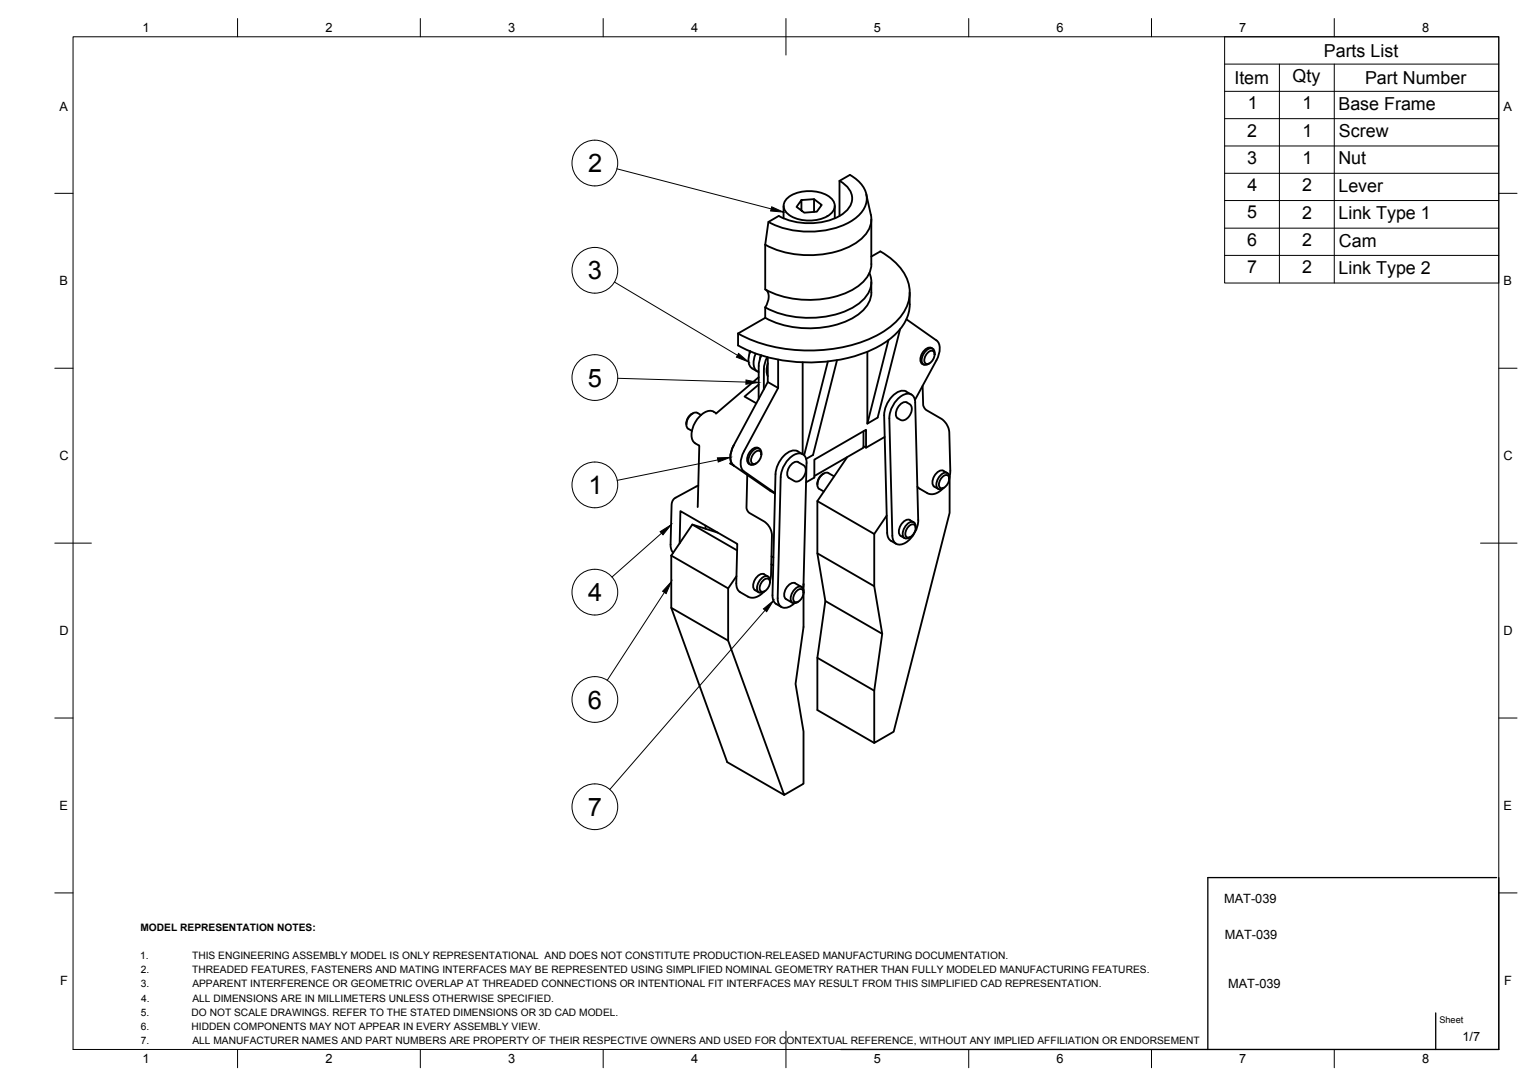
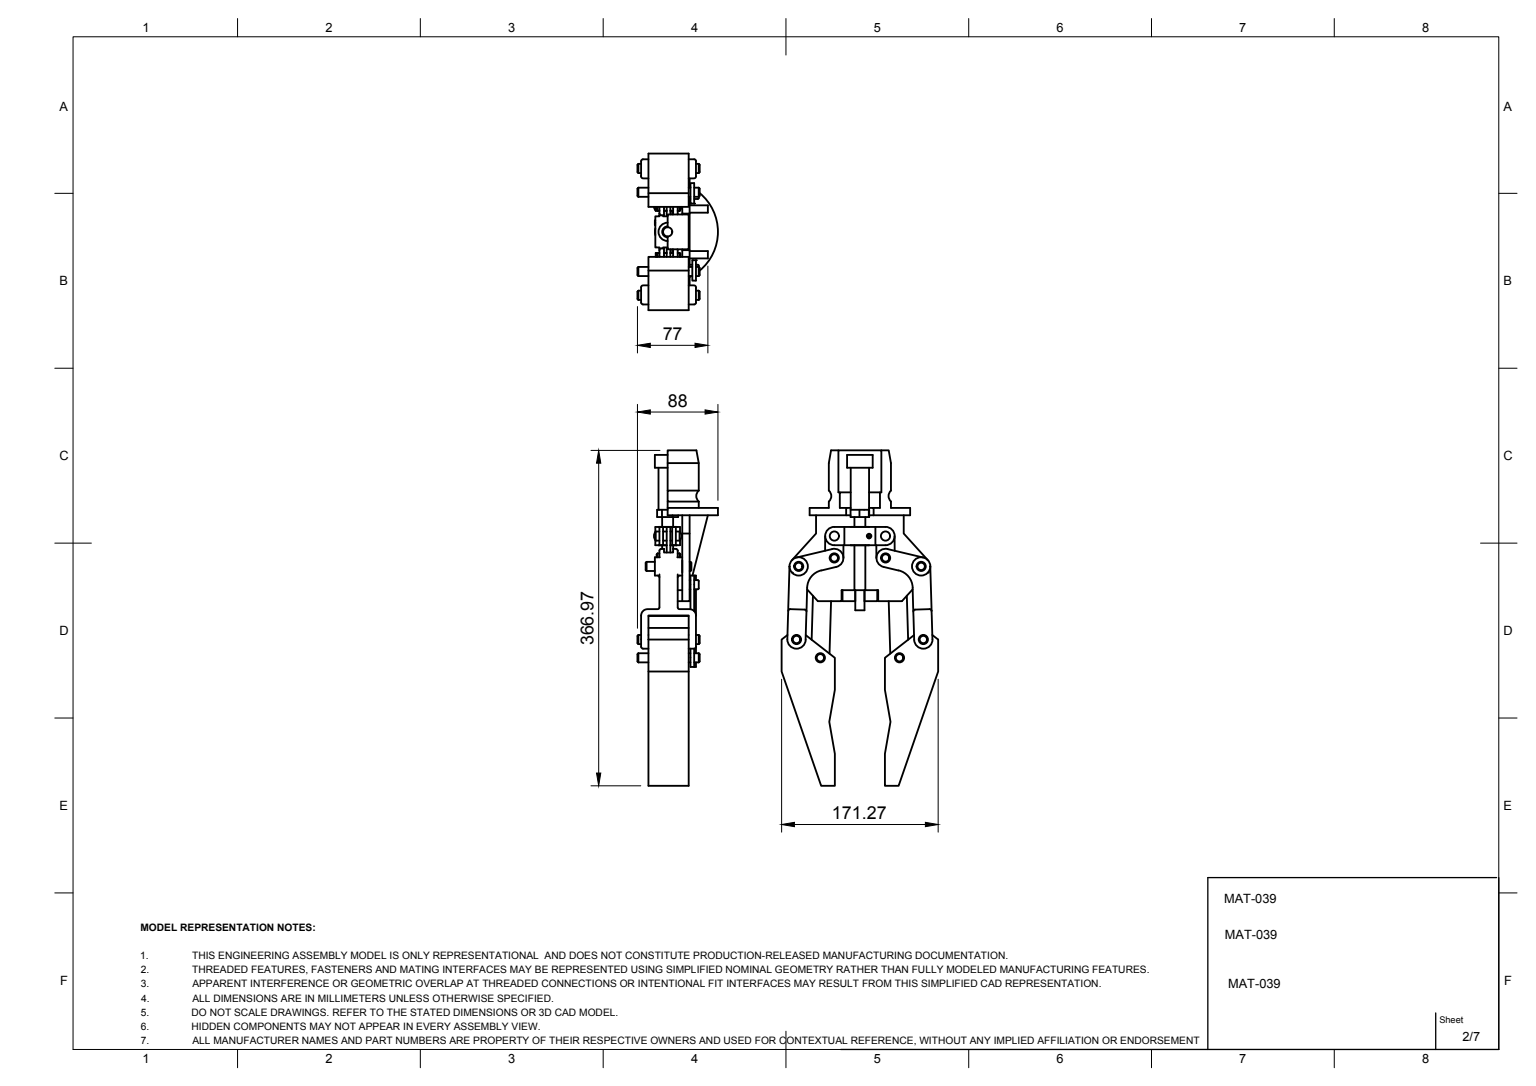
ISO-10303-21;
HEADER;
/* Generated by software containing ST-Developer
 * from STEP Tools, Inc. (www.steptools.com) 
 */

FILE_DESCRIPTION(
/* description */ ('STEP AP214'),
/* implementation_level */ '2;1');

FILE_NAME(
/* name */ 'MAT-039.step',
/* time_stamp */ '2026-11-14T21:46:24-08:00',
/* author */ (''),
/* organization */ (''),
/* preprocessor_version */ 'ST-DEVELOPER v20.2',
/* originating_system */ 'Autodesk Translation Framework v15.17.0.0',
/* authorisation */ '');

FILE_SCHEMA (('AUTOMOTIVE_DESIGN { 1 0 10303 214 3 1 1 }'));
ENDSEC;

DATA;
#10=MECHANICAL_DESIGN_GEOMETRIC_PRESENTATION_REPRESENTATION('',(#89,#90,
#91,#92,#93,#94,#95),#7783);
#11=(
BOUNDED_SURFACE()
B_SPLINE_SURFACE(3,2,((#7242,#7243,#7244),(#7245,#7246,#7247),(#7248,#7249,
#7250),(#7251,#7252,#7253),(#7254,#7255,#7256),(#7257,#7258,#7259),(#7260,
#7261,#7262),(#7263,#7264,#7265),(#7266,#7267,#7268),(#7269,#7270,#7271),
(#7272,#7273,#7274),(#7275,#7276,#7277),(#7278,#7279,#7280),(#7281,#7282,
#7283)),.UNSPECIFIED.,.F.,.F.,.F.)
B_SPLINE_SURFACE_WITH_KNOTS((4,2,2,2,2,2,4),(3,3),(0.00201286221565559,
0.00340012561105001,0.00476544226438698,0.00613075891772395,0.00749607557106092,
0.0102267088777349,0.0129573421844088),(0.,1.00002194674206),
 .UNSPECIFIED.)
GEOMETRIC_REPRESENTATION_ITEM()
RATIONAL_B_SPLINE_SURFACE(((1.,0.706119316799645,1.0000128994471),(1.,0.726784777924549,
1.00001199236801),(1.,0.747777874428932,1.00001107090786),(1.,0.788599708818028,
1.00000927909532),(1.,0.808519289419434,1.00000840475553),(1.,0.845529525851375,
1.0000067802473),(1.,0.862790936611022,1.00000602258384),(1.,0.894561465950779,
1.00000462806462),(1.,0.909105255838781,1.00000398968701),(1.,0.948117278028828,
1.00000227731343),(1.,0.967426794359605,1.00000142975148),(1.,0.993377057003404,
1.00000029070404),(1.,0.999996114407628,1.00000000017055),(1.,1.,1.)))
REPRESENTATION_ITEM('')
SURFACE()
);
#12=(
BOUNDED_SURFACE()
B_SPLINE_SURFACE(3,2,((#7288,#7289,#7290),(#7291,#7292,#7293),(#7294,#7295,
#7296),(#7297,#7298,#7299),(#7300,#7301,#7302),(#7303,#7304,#7305),(#7306,
#7307,#7308),(#7309,#7310,#7311),(#7312,#7313,#7314),(#7315,#7316,#7317),
(#7318,#7319,#7320),(#7321,#7322,#7323),(#7324,#7325,#7326),(#7327,#7328,
#7329)),.UNSPECIFIED.,.F.,.F.,.F.)
B_SPLINE_SURFACE_WITH_KNOTS((4,2,2,2,2,2,4),(3,3),(0.00201286221604104,
0.00340012561105,0.00476544226438698,0.00613075891772395,0.00749607557106092,
0.0102267088777349,0.0129573421844088),(-2.19467416719971E-5,1.00004202921769),
 .UNSPECIFIED.)
GEOMETRIC_REPRESENTATION_ITEM()
RATIONAL_B_SPLINE_SURFACE(((1.00001289944687,0.706106964970707,1.00002470364651),
(1.0000119923678,0.726773294662226,1.00002296650529),(1.00001107090767,
0.747767273503531,1.00002120182301),(1.00000927909516,0.788590823634209,
1.00001777033457),(1.00000840475538,0.808511241458396,1.00001609589217),
(1.00000678024718,0.845523033435795,1.00001298480712),(1.00000602258374,
0.862785169694921,1.00001153381081),(1.00000462806454,0.894557034354464,
1.00000886317619),(1.00000398968694,0.909101435519961,1.00000764062341),
(1.00000227731339,0.948115097390828,1.00000436126801),(1.00000142975146,
0.967425425303272,1.00000273810769),(1.00000029070404,0.993376778640135,
1.00000055672541),(1.00000000017055,0.999996114244353,1.00000000032662),
(1.,1.,1.)))
REPRESENTATION_ITEM('')
SURFACE()
);
#13=(
BOUNDED_SURFACE()
B_SPLINE_SURFACE(3,2,((#7444,#7445,#7446),(#7447,#7448,#7449),(#7450,#7451,
#7452),(#7453,#7454,#7455),(#7456,#7457,#7458),(#7459,#7460,#7461),(#7462,
#7463,#7464),(#7465,#7466,#7467),(#7468,#7469,#7470),(#7471,#7472,#7473),
(#7474,#7475,#7476),(#7477,#7478,#7479),(#7480,#7481,#7482),(#7483,#7484,
#7485)),.UNSPECIFIED.,.F.,.F.,.F.)
B_SPLINE_SURFACE_WITH_KNOTS((4,2,2,2,2,2,4),(3,3),(0.00203480895771304,
0.00340012561105001,0.00476544226438698,0.00613075891772395,0.00749607557106092,
0.0102267088777349,0.0129573421844088),(0.,1.),.UNSPECIFIED.)
GEOMETRIC_REPRESENTATION_ITEM()
RATIONAL_B_SPLINE_SURFACE(((1.,0.707106781186548,1.),(1.,0.727454883115531,
1.),(1.,0.748108881352396,1.),(1.,0.788604348263869,1.),(1.,0.808523491704972,
1.),(1.,0.845532915900626,1.),(1.,0.862793947836832,1.),(1.,0.89456377993233,
1.),(1.,0.909107250638557,1.),(1.,0.948118416660453,1.),(1.,0.967427509219659,
1.),(1.,0.993377202352236,1.),(1.,0.999996114492902,1.),(1.,1.,1.)))
REPRESENTATION_ITEM('')
SURFACE()
);
#14=(
BOUNDED_SURFACE()
B_SPLINE_SURFACE(3,2,((#7492,#7493,#7494),(#7495,#7496,#7497),(#7498,#7499,
#7500),(#7501,#7502,#7503),(#7504,#7505,#7506),(#7507,#7508,#7509),(#7510,
#7511,#7512),(#7513,#7514,#7515),(#7516,#7517,#7518),(#7519,#7520,#7521),
(#7522,#7523,#7524),(#7525,#7526,#7527),(#7528,#7529,#7530),(#7531,#7532,
#7533)),.UNSPECIFIED.,.F.,.F.,.F.)
B_SPLINE_SURFACE_WITH_KNOTS((4,2,2,2,2,2,4),(3,3),(0.00203480895771304,
0.00340012561105001,0.00476544226438698,0.00613075891772395,0.00749607557106092,
0.0102267088777349,0.0129573421844088),(-4.20282077345397E-5,1.),
 .UNSPECIFIED.)
GEOMETRIC_REPRESENTATION_ITEM()
RATIONAL_B_SPLINE_SURFACE(((1.0000246205888,0.707094471409503,1.),(1.00002291012841,
0.727443428532761,1.),(1.00002117395439,0.74809829482011,1.),(1.00001776990754,
0.788595463683529,1.),(1.00001609550537,0.808515444290505,1.),(1.00001298449509,
0.845526423925928,1.),(1.00001153353364,0.862788181312395,1.),(1.0000088629632,
0.894559348636945,1.),(1.0000076404398,0.909103430579154,1.),(1.00000436116321,
0.948116236170593,1.),(1.00000273804189,0.967426140256249,1.),(1.00000055671203,
0.99337692400792,1.),(1.00000000032662,0.999996114329601,1.),(1.,1.,1.)))
REPRESENTATION_ITEM('')
SURFACE()
);
#15=B_SPLINE_CURVE_WITH_KNOTS('',3,(#6784,#6785,#6786,#6787,#6788,#6789,
#6790,#6791,#6792,#6793,#6794,#6795,#6796,#6797,#6798,#6799,#6800,#6801,
#6802,#6803,#6804,#6805,#6806,#6807,#6808,#6809,#6810,#6811,#6812,#6813,
#6814,#6815,#6816,#6817,#6818,#6819,#6820,#6821,#6822,#6823,#6824,#6825,
#6826,#6827,#6828,#6829,#6830,#6831,#6832),.UNSPECIFIED.,.F.,.F.,(4,3,3,
3,3,3,3,3,3,3,3,3,3,3,3,3,4),(0.,0.000463967413666575,0.000954777042109378,
0.00114718345131556,0.00157257184718515,0.0019889538699822,0.00230336685082165,
0.00277738225277823,0.00314514369437031,0.0034731976359017,0.00393142961796289,
0.00434870227875263,0.00465308895983082,0.00471771554155546,0.00539019410311121,
0.00607303876857302,0.00629028738874061),.UNSPECIFIED.);
#16=B_SPLINE_CURVE_WITH_KNOTS('',3,(#6834,#6835,#6836,#6837,#6838,#6839),
 .UNSPECIFIED.,.F.,.F.,(4,2,4),(0.00629028738874061,0.0078707452346593,
0.00945120308057799),.UNSPECIFIED.);
#17=B_SPLINE_CURVE_WITH_KNOTS('',3,(#6843,#6844,#6845,#6846,#6847,#6848),
 .UNSPECIFIED.,.F.,.F.,(4,2,4),(-2.00176139701977E-5,0.00156468827612987,
0.00314939416622993),.UNSPECIFIED.);
#18=B_SPLINE_CURVE_WITH_KNOTS('',3,(#6849,#6850,#6851,#6852,#6853,#6854,
#6855,#6856,#6857,#6858,#6859,#6860,#6861,#6862,#6863,#6864,#6865,#6866,
#6867,#6868,#6869,#6870,#6871,#6872,#6873,#6874,#6875,#6876,#6877,#6878,
#6879,#6880,#6881,#6882,#6883,#6884,#6885,#6886,#6887,#6888,#6889,#6890,
#6891,#6892,#6893,#6894,#6895,#6896,#6897),.UNSPECIFIED.,.F.,.F.,(4,3,3,
3,3,3,3,3,3,3,3,3,3,3,3,3,4),(0.00314939416622993,0.00383486824301925,0.00450997916923667,
0.00472621979976512,0.00479102119555099,0.00520942257342087,0.00551463261653271,
0.00597410411013286,0.0063030454333003,0.0067783430407421,0.00714709927223923,
0.00756460760297828,0.00787987106683548,0.0083064101327715,0.00880180611055996,
0.00926887465145742,0.00945669670037066),.UNSPECIFIED.);
#19=B_SPLINE_CURVE_WITH_KNOTS('',3,(#6902,#6903,#6904,#6905,#6906,#6907,
#6908,#6909,#6910,#6911,#6912,#6913,#6914,#6915,#6916,#6917,#6918,#6919,
#6920,#6921,#6922,#6923,#6924,#6925,#6926,#6927,#6928,#6929,#6930,#6931,
#6932,#6933,#6934,#6935,#6936,#6937,#6938,#6939,#6940,#6941,#6942,#6943,
#6944,#6945,#6946,#6947,#6948,#6949,#6950,#6951,#6952,#6953,#6954,#6955,
#6956,#6957,#6958,#6959,#6960,#6961,#6962,#6963,#6964,#6965,#6966,#6967,
#6968),.UNSPECIFIED.,.F.,.F.,(4,3,3,3,3,3,3,3,3,3,3,3,3,3,3,3,3,3,3,3,3,
3,4),(0.,0.000573434007013873,0.00114686801402775,0.00118140038507225,0.00174268388294295,
0.00230396738081366,0.0023628007701445,0.00306787423031747,0.00347315409373973,
0.00354420115521674,0.0040039106218915,0.0044814901760133,0.00465309204256514,
0.00472560154028899,0.00565974635025426,0.00664141956317292,0.00704595844743703,
0.00708840231043349,0.0077443311007397,0.00826980269550574,0.00881956648446386,
0.00937303729633357,0.00945120308057799),.UNSPECIFIED.);
#20=B_SPLINE_CURVE_WITH_KNOTS('',3,(#6972,#6973,#6974,#6975,#6976,#6977,
#6978,#6979,#6980,#6981,#6982,#6983,#6984,#6985,#6986,#6987,#6988,#6989,
#6990,#6991,#6992,#6993,#6994,#6995,#6996,#6997,#6998,#6999,#7000,#7001,
#7002,#7003,#7004,#7005,#7006,#7007,#7008,#7009,#7010,#7011,#7012,#7013,
#7014,#7015,#7016,#7017,#7018,#7019,#7020,#7021,#7022,#7023,#7024,#7025,
#7026,#7027,#7028,#7029,#7030,#7031,#7032,#7033,#7034,#7035),
 .UNSPECIFIED.,.F.,.F.,(4,3,3,3,3,3,3,3,3,3,3,3,3,3,3,3,3,3,3,3,3,4),(-2.00176139701506E-5,
0.000743071051629322,0.00154611600812219,0.00230505274395684,0.00234916096461506,
0.00239167902346657,0.00338088357647153,0.00432175791491912,0.00471833954320027,
0.00479101813919611,0.0052714217586875,0.00573373183999769,0.00590292883249288,
0.00597414776682822,0.00668110904687163,0.00708751812178548,0.00714649712036357,
0.00770930226572083,0.00827210741107809,0.00830672642201829,0.00888171156119449,
0.0094566967003707),.UNSPECIFIED.);
#21=B_SPLINE_CURVE_WITH_KNOTS('',3,(#7224,#7225,#7226,#7227,#7228,#7229,
#7230,#7231,#7232,#7233,#7234,#7235,#7236,#7237,#7238,#7239),
 .UNSPECIFIED.,.F.,.F.,(4,2,2,2,2,2,2,4),(0.,0.0011867209290651,0.0023734418581302,
0.00356016278719531,0.00474688371626041,0.00712032557439061,0.00830704650345571,
0.00949376743252081),.UNSPECIFIED.);
#22=B_SPLINE_CURVE_WITH_KNOTS('',3,(#7330,#7331,#7332,#7333,#7334,#7335,
#7336,#7337,#7338,#7339,#7340,#7341,#7342,#7343,#7344,#7345),
 .UNSPECIFIED.,.F.,.F.,(4,2,2,2,2,2,2,4),(0.,0.0011867209290651,0.00237344185813019,
0.00356016278719529,0.00474688371626039,0.00712032557439059,0.00830704650345569,
0.00949376743252079),.UNSPECIFIED.);
#23=B_SPLINE_CURVE_WITH_KNOTS('',3,(#7372,#7373,#7374,#7375,#7376,#7377,
#7378,#7379,#7380,#7381,#7382,#7383,#7384,#7385,#7386,#7387,#7388,#7389,
#7390,#7391,#7392,#7393,#7394,#7395,#7396,#7397,#7398,#7399,#7400,#7401,
#7402,#7403,#7404,#7405,#7406,#7407,#7408,#7409,#7410,#7411,#7412,#7413,
#7414,#7415,#7416,#7417,#7418,#7419,#7420,#7421,#7422,#7423,#7424,#7425,
#7426,#7427,#7428,#7429,#7430,#7431,#7432,#7433,#7434,#7435,#7436,#7437,
#7438,#7439,#7440,#7441),.UNSPECIFIED.,.F.,.F.,(4,3,3,3,3,3,3,3,3,3,3,3,
3,3,3,3,3,3,3,3,3,3,3,4),(-2.20338883785527E-5,0.000642558597019686,0.00116395721593939,
0.00201707586197036,0.00234994832025733,0.00244440929736401,0.00317109830627835,
0.00387836420487405,0.00455999932782322,0.00472193052889321,0.00487208598317901,
0.00547292850863629,0.00607377103409357,0.00663117903387144,0.00709391273752908,
0.00724862880926105,0.00759056213579682,0.00791199062197989,0.0082104406191189,
0.00827990384184702,0.00838782827049795,0.00882409089832456,0.00926054923459336,
0.00946589494616496),.UNSPECIFIED.);
#24=B_SPLINE_CURVE_WITH_KNOTS('',3,(#7534,#7535,#7536,#7537,#7538,#7539,
#7540,#7541,#7542,#7543,#7544,#7545,#7546,#7547,#7548,#7549,#7550,#7551,
#7552,#7553,#7554,#7555,#7556,#7557,#7558,#7559,#7560,#7561,#7562,#7563,
#7564,#7565,#7566,#7567,#7568,#7569,#7570,#7571,#7572,#7573,#7574,#7575,
#7576,#7577,#7578,#7579,#7580,#7581,#7582,#7583,#7584,#7585,#7586,#7587,
#7588,#7589,#7590,#7591,#7592,#7593,#7594,#7595,#7596,#7597,#7598,#7599,
#7600,#7601,#7602,#7603),.UNSPECIFIED.,.F.,.F.,(4,3,3,3,3,3,3,3,3,3,3,3,
3,3,3,3,3,3,3,3,3,3,3,4),(-2.20338883785244E-5,0.000642558597506865,0.00116395721593941,
0.00201707586185835,0.00234994832025735,0.00244440929736402,0.00317109830623264,
0.00387836420476937,0.0045599993276549,0.00472193052889323,0.00487208598317904,
0.00547292850863634,0.00607377103409363,0.00663117903387409,0.00709391273752911,
0.00724862880926107,0.00759056213580112,0.00791199062198886,0.00821044061913349,
0.00827990384184705,0.00838782827049793,0.00882409089835773,0.00926054923468115,
0.00946589494616499),.UNSPECIFIED.);
#25=SPHERICAL_SURFACE('',#4400,7.25);
#26=SPHERICAL_SURFACE('',#4410,7.25);
#27=ITEM_DEFINED_TRANSFORMATION($,$,#4251,#4337);
#28=ITEM_DEFINED_TRANSFORMATION($,$,#4250,#4701);
#29=ITEM_DEFINED_TRANSFORMATION($,$,#4338,#4702);
#30=ITEM_DEFINED_TRANSFORMATION($,$,#4381,#4703);
#31=ITEM_DEFINED_TRANSFORMATION($,$,#4478,#4704);
#32=ITEM_DEFINED_TRANSFORMATION($,$,#4461,#4705);
#33=ITEM_DEFINED_TRANSFORMATION($,$,#4663,#4706);
#34=ITEM_DEFINED_TRANSFORMATION($,$,#4646,#4707);
#35=ITEM_DEFINED_TRANSFORMATION($,$,#4461,#4708);
#36=ITEM_DEFINED_TRANSFORMATION($,$,#4478,#4709);
#37=ITEM_DEFINED_TRANSFORMATION($,$,#4646,#4710);
#38=ITEM_DEFINED_TRANSFORMATION($,$,#4663,#4711);
#39=(
REPRESENTATION_RELATIONSHIP($,$,#7820,#7819)
REPRESENTATION_RELATIONSHIP_WITH_TRANSFORMATION(#27)
SHAPE_REPRESENTATION_RELATIONSHIP()
);
#40=(
REPRESENTATION_RELATIONSHIP($,$,#7819,#7818)
REPRESENTATION_RELATIONSHIP_WITH_TRANSFORMATION(#28)
SHAPE_REPRESENTATION_RELATIONSHIP()
);
#41=(
REPRESENTATION_RELATIONSHIP($,$,#7821,#7818)
REPRESENTATION_RELATIONSHIP_WITH_TRANSFORMATION(#29)
SHAPE_REPRESENTATION_RELATIONSHIP()
);
#42=(
REPRESENTATION_RELATIONSHIP($,$,#7822,#7818)
REPRESENTATION_RELATIONSHIP_WITH_TRANSFORMATION(#30)
SHAPE_REPRESENTATION_RELATIONSHIP()
);
#43=(
REPRESENTATION_RELATIONSHIP($,$,#7824,#7818)
REPRESENTATION_RELATIONSHIP_WITH_TRANSFORMATION(#31)
SHAPE_REPRESENTATION_RELATIONSHIP()
);
#44=(
REPRESENTATION_RELATIONSHIP($,$,#7823,#7818)
REPRESENTATION_RELATIONSHIP_WITH_TRANSFORMATION(#32)
SHAPE_REPRESENTATION_RELATIONSHIP()
);
#45=(
REPRESENTATION_RELATIONSHIP($,$,#7826,#7818)
REPRESENTATION_RELATIONSHIP_WITH_TRANSFORMATION(#33)
SHAPE_REPRESENTATION_RELATIONSHIP()
);
#46=(
REPRESENTATION_RELATIONSHIP($,$,#7825,#7818)
REPRESENTATION_RELATIONSHIP_WITH_TRANSFORMATION(#34)
SHAPE_REPRESENTATION_RELATIONSHIP()
);
#47=(
REPRESENTATION_RELATIONSHIP($,$,#7823,#7818)
REPRESENTATION_RELATIONSHIP_WITH_TRANSFORMATION(#35)
SHAPE_REPRESENTATION_RELATIONSHIP()
);
#48=(
REPRESENTATION_RELATIONSHIP($,$,#7824,#7818)
REPRESENTATION_RELATIONSHIP_WITH_TRANSFORMATION(#36)
SHAPE_REPRESENTATION_RELATIONSHIP()
);
#49=(
REPRESENTATION_RELATIONSHIP($,$,#7825,#7818)
REPRESENTATION_RELATIONSHIP_WITH_TRANSFORMATION(#37)
SHAPE_REPRESENTATION_RELATIONSHIP()
);
#50=(
REPRESENTATION_RELATIONSHIP($,$,#7826,#7818)
REPRESENTATION_RELATIONSHIP_WITH_TRANSFORMATION(#38)
SHAPE_REPRESENTATION_RELATIONSHIP()
);
#51=CONTEXT_DEPENDENT_SHAPE_REPRESENTATION(#39,#7800);
#52=CONTEXT_DEPENDENT_SHAPE_REPRESENTATION(#40,#7807);
#53=CONTEXT_DEPENDENT_SHAPE_REPRESENTATION(#41,#7808);
#54=CONTEXT_DEPENDENT_SHAPE_REPRESENTATION(#42,#7809);
#55=CONTEXT_DEPENDENT_SHAPE_REPRESENTATION(#43,#7810);
#56=CONTEXT_DEPENDENT_SHAPE_REPRESENTATION(#44,#7811);
#57=CONTEXT_DEPENDENT_SHAPE_REPRESENTATION(#45,#7812);
#58=CONTEXT_DEPENDENT_SHAPE_REPRESENTATION(#46,#7813);
#59=CONTEXT_DEPENDENT_SHAPE_REPRESENTATION(#47,#7814);
#60=CONTEXT_DEPENDENT_SHAPE_REPRESENTATION(#48,#7815);
#61=CONTEXT_DEPENDENT_SHAPE_REPRESENTATION(#49,#7816);
#62=CONTEXT_DEPENDENT_SHAPE_REPRESENTATION(#50,#7817);
#63=NEXT_ASSEMBLY_USAGE_OCCURRENCE('Body 1:1','Body 1:1','Body 1:1',#7829,
#7830,'Body 1:1');
#64=NEXT_ASSEMBLY_USAGE_OCCURRENCE('Base Frame:1','Base Frame:1',
'Base Frame:1',#7828,#7829,'Base Frame:1');
#65=NEXT_ASSEMBLY_USAGE_OCCURRENCE('Screw:1','Screw:1','Screw:1',#7828,
#7831,'Screw:1');
#66=NEXT_ASSEMBLY_USAGE_OCCURRENCE('Nut:1','Nut:1','Nut:1',#7828,#7832,
'Nut:1');
#67=NEXT_ASSEMBLY_USAGE_OCCURRENCE('Lever:1','Lever:1','Lever:1',#7828,
#7834,'Lever:1');
#68=NEXT_ASSEMBLY_USAGE_OCCURRENCE('Link Type 1:1','Link Type 1:1',
'Link Type 1:1',#7828,#7833,'Link Type 1:1');
#69=NEXT_ASSEMBLY_USAGE_OCCURRENCE('Cam:1','Cam:1','Cam:1',#7828,#7836,
'Cam:1');
#70=NEXT_ASSEMBLY_USAGE_OCCURRENCE('Link Type 2:1','Link Type 2:1',
'Link Type 2:1',#7828,#7835,'Link Type 2:1');
#71=NEXT_ASSEMBLY_USAGE_OCCURRENCE('Link Type 1:2','Link Type 1:2',
'Link Type 1:2',#7828,#7833,'Link Type 1:2');
#72=NEXT_ASSEMBLY_USAGE_OCCURRENCE('Lever:2','Lever:2','Lever:2',#7828,
#7834,'Lever:2');
#73=NEXT_ASSEMBLY_USAGE_OCCURRENCE('Link Type 2:2','Link Type 2:2',
'Link Type 2:2',#7828,#7835,'Link Type 2:2');
#74=NEXT_ASSEMBLY_USAGE_OCCURRENCE('Cam:2','Cam:2','Cam:2',#7828,#7836,
'Cam:2');
#75=SHAPE_REPRESENTATION_RELATIONSHIP('SRR','None',#7820,#82);
#76=SHAPE_REPRESENTATION_RELATIONSHIP('SRR','None',#7821,#83);
#77=SHAPE_REPRESENTATION_RELATIONSHIP('SRR','None',#7822,#84);
#78=SHAPE_REPRESENTATION_RELATIONSHIP('SRR','None',#7823,#85);
#79=SHAPE_REPRESENTATION_RELATIONSHIP('SRR','None',#7824,#86);
#80=SHAPE_REPRESENTATION_RELATIONSHIP('SRR','None',#7825,#87);
#81=SHAPE_REPRESENTATION_RELATIONSHIP('SRR','None',#7826,#88);
#82=ADVANCED_BREP_SHAPE_REPRESENTATION('',(#96),#7776);
#83=ADVANCED_BREP_SHAPE_REPRESENTATION('',(#97),#7777);
#84=ADVANCED_BREP_SHAPE_REPRESENTATION('',(#98),#7778);
#85=ADVANCED_BREP_SHAPE_REPRESENTATION('',(#99),#7779);
#86=ADVANCED_BREP_SHAPE_REPRESENTATION('',(#100),#7780);
#87=ADVANCED_BREP_SHAPE_REPRESENTATION('',(#101),#7781);
#88=ADVANCED_BREP_SHAPE_REPRESENTATION('',(#102),#7782);
#89=STYLED_ITEM('',(#7868),#96);
#90=STYLED_ITEM('',(#7869),#97);
#91=STYLED_ITEM('',(#7869),#98);
#92=STYLED_ITEM('',(#7870),#99);
#93=STYLED_ITEM('',(#7868),#100);
#94=STYLED_ITEM('',(#7871),#101);
#95=STYLED_ITEM('',(#7871),#102);
#96=MANIFOLD_SOLID_BREP('Body1',#4164);
#97=MANIFOLD_SOLID_BREP('Body1',#4165);
#98=MANIFOLD_SOLID_BREP('Body1',#4166);
#99=MANIFOLD_SOLID_BREP('Body1',#4167);
#100=MANIFOLD_SOLID_BREP('Body1',#4168);
#101=MANIFOLD_SOLID_BREP('Body1',#4169);
#102=MANIFOLD_SOLID_BREP('Body1',#4170);
#103=CONICAL_SURFACE('',#4303,34.,0.176708856070037);
#104=CONICAL_SURFACE('',#4479,3.99999999999998,0.785398163397453);
#105=CONICAL_SURFACE('',#4482,3.99999999999998,0.785398163397454);
#106=CONICAL_SURFACE('',#4485,5.,0.785398163397443);
#107=CONICAL_SURFACE('',#4489,5.,0.785398163397443);
#108=CONICAL_SURFACE('',#4664,5.,0.785398163397445);
#109=CONICAL_SURFACE('',#4668,5.,0.785398163397445);
#110=CONICAL_SURFACE('',#4672,3.99999999999998,0.785398163397453);
#111=CONICAL_SURFACE('',#4675,3.99999999999998,0.785398163397453);
#112=FACE_BOUND('',#1344,.T.);
#113=FACE_BOUND('',#1345,.T.);
#114=FACE_BOUND('',#1346,.T.);
#115=FACE_BOUND('',#1347,.T.);
#116=FACE_BOUND('',#1352,.T.);
#117=FACE_BOUND('',#1359,.T.);
#118=FACE_BOUND('',#1360,.T.);
#119=FACE_BOUND('',#1393,.T.);
#120=FACE_BOUND('',#1395,.T.);
#121=FACE_BOUND('',#1404,.T.);
#122=FACE_BOUND('',#1419,.T.);
#123=FACE_BOUND('',#1436,.T.);
#124=FACE_BOUND('',#1438,.T.);
#125=FACE_BOUND('',#1440,.T.);
#126=FACE_BOUND('',#1442,.T.);
#127=FACE_BOUND('',#1444,.T.);
#128=FACE_BOUND('',#1446,.T.);
#129=FACE_BOUND('',#1448,.T.);
#130=FACE_BOUND('',#1450,.T.);
#131=FACE_BOUND('',#1452,.T.);
#132=FACE_BOUND('',#1454,.T.);
#133=FACE_BOUND('',#1457,.T.);
#134=FACE_BOUND('',#1462,.T.);
#135=FACE_BOUND('',#1472,.T.);
#136=FACE_BOUND('',#1474,.T.);
#137=FACE_BOUND('',#1483,.T.);
#138=FACE_BOUND('',#1484,.T.);
#139=FACE_BOUND('',#1486,.T.);
#140=FACE_BOUND('',#1487,.T.);
#141=FACE_BOUND('',#1509,.T.);
#142=FACE_BOUND('',#1516,.T.);
#143=FACE_BOUND('',#1520,.T.);
#144=FACE_BOUND('',#1523,.T.);
#145=FACE_BOUND('',#1526,.T.);
#146=FACE_BOUND('',#1528,.T.);
#147=FACE_BOUND('',#1530,.T.);
#148=FACE_BOUND('',#1533,.T.);
#149=FACE_BOUND('',#1535,.T.);
#150=FACE_BOUND('',#1538,.T.);
#151=FACE_BOUND('',#1584,.T.);
#152=FACE_BOUND('',#1585,.T.);
#153=FACE_BOUND('',#1587,.T.);
#154=FACE_BOUND('',#1588,.T.);
#155=FACE_BOUND('',#1601,.T.);
#156=FACE_BOUND('',#1602,.T.);
#157=FACE_BOUND('',#1604,.T.);
#158=FACE_BOUND('',#1605,.T.);
#159=PLANE('',#4294);
#160=PLANE('',#4297);
#161=PLANE('',#4298);
#162=PLANE('',#4299);
#163=PLANE('',#4300);
#164=PLANE('',#4301);
#165=PLANE('',#4304);
#166=PLANE('',#4305);
#167=PLANE('',#4306);
#168=PLANE('',#4307);
#169=PLANE('',#4310);
#170=PLANE('',#4311);
#171=PLANE('',#4313);
#172=PLANE('',#4314);
#173=PLANE('',#4315);
#174=PLANE('',#4317);
#175=PLANE('',#4318);
#176=PLANE('',#4319);
#177=PLANE('',#4320);
#178=PLANE('',#4321);
#179=PLANE('',#4322);
#180=PLANE('',#4323);
#181=PLANE('',#4324);
#182=PLANE('',#4325);
#183=PLANE('',#4326);
#184=PLANE('',#4327);
#185=PLANE('',#4328);
#186=PLANE('',#4329);
#187=PLANE('',#4330);
#188=PLANE('',#4331);
#189=PLANE('',#4332);
#190=PLANE('',#4333);
#191=PLANE('',#4334);
#192=PLANE('',#4335);
#193=PLANE('',#4336);
#194=PLANE('',#4357);
#195=PLANE('',#4358);
#196=PLANE('',#4359);
#197=PLANE('',#4360);
#198=PLANE('',#4361);
#199=PLANE('',#4362);
#200=PLANE('',#4363);
#201=PLANE('',#4364);
#202=PLANE('',#4365);
#203=PLANE('',#4366);
#204=PLANE('',#4367);
#205=PLANE('',#4368);
#206=PLANE('',#4369);
#207=PLANE('',#4370);
#208=PLANE('',#4371);
#209=PLANE('',#4372);
#210=PLANE('',#4373);
#211=PLANE('',#4374);
#212=PLANE('',#4375);
#213=PLANE('',#4376);
#214=PLANE('',#4377);
#215=PLANE('',#4378);
#216=PLANE('',#4379);
#217=PLANE('',#4380);
#218=PLANE('',#4423);
#219=PLANE('',#4424);
#220=PLANE('',#4425);
#221=PLANE('',#4427);
#222=PLANE('',#4429);
#223=PLANE('',#4431);
#224=PLANE('',#4433);
#225=PLANE('',#4435);
#226=PLANE('',#4437);
#227=PLANE('',#4439);
#228=PLANE('',#4441);
#229=PLANE('',#4442);
#230=PLANE('',#4443);
#231=PLANE('',#4444);
#232=PLANE('',#4445);
#233=PLANE('',#4446);
#234=PLANE('',#4447);
#235=PLANE('',#4448);
#236=PLANE('',#4453);
#237=PLANE('',#4454);
#238=PLANE('',#4455);
#239=PLANE('',#4456);
#240=PLANE('',#4457);
#241=PLANE('',#4458);
#242=PLANE('',#4459);
#243=PLANE('',#4460);
#244=PLANE('',#4471);
#245=PLANE('',#4473);
#246=PLANE('',#4475);
#247=PLANE('',#4477);
#248=PLANE('',#4536);
#249=PLANE('',#4539);
#250=PLANE('',#4540);
#251=PLANE('',#4544);
#252=PLANE('',#4549);
#253=PLANE('',#4554);
#254=PLANE('',#4557);
#255=PLANE('',#4558);
#256=PLANE('',#4559);
#257=PLANE('',#4560);
#258=PLANE('',#4561);
#259=PLANE('',#4562);
#260=PLANE('',#4563);
#261=PLANE('',#4566);
#262=PLANE('',#4571);
#263=PLANE('',#4572);
#264=PLANE('',#4573);
#265=PLANE('',#4574);
#266=PLANE('',#4642);
#267=PLANE('',#4643);
#268=PLANE('',#4644);
#269=PLANE('',#4645);
#270=PLANE('',#4656);
#271=PLANE('',#4658);
#272=PLANE('',#4660);
#273=PLANE('',#4662);
#274=PLANE('',#4686);
#275=PLANE('',#4687);
#276=PLANE('',#4688);
#277=PLANE('',#4689);
#278=PLANE('',#4690);
#279=PLANE('',#4691);
#280=PLANE('',#4692);
#281=PLANE('',#4693);
#282=PLANE('',#4694);
#283=PLANE('',#4695);
#284=PLANE('',#4696);
#285=PLANE('',#4697);
#286=PLANE('',#4698);
#287=PLANE('',#4699);
#288=PLANE('',#4700);
#289=LINE('',#6018,#648);
#290=LINE('',#6028,#649);
#291=LINE('',#6034,#650);
#292=LINE('',#6037,#651);
#293=LINE('',#6042,#652);
#294=LINE('',#6048,#653);
#295=LINE('',#6055,#654);
#296=LINE('',#6058,#655);
#297=LINE('',#6064,#656);
#298=LINE('',#6067,#657);
#299=LINE('',#6073,#658);
#300=LINE('',#6076,#659);
#301=LINE('',#6082,#660);
#302=LINE('',#6085,#661);
#303=LINE('',#6090,#662);
#304=LINE('',#6091,#663);
#305=LINE('',#6094,#664);
#306=LINE('',#6097,#665);
#307=LINE('',#6101,#666);
#308=LINE('',#6103,#667);
#309=LINE('',#6105,#668);
#310=LINE('',#6107,#669);
#311=LINE('',#6109,#670);
#312=LINE('',#6113,#671);
#313=LINE('',#6115,#672);
#314=LINE('',#6117,#673);
#315=LINE('',#6119,#674);
#316=LINE('',#6121,#675);
#317=LINE('',#6123,#676);
#318=LINE('',#6125,#677);
#319=LINE('',#6127,#678);
#320=LINE('',#6129,#679);
#321=LINE('',#6131,#680);
#322=LINE('',#6133,#681);
#323=LINE('',#6135,#682);
#324=LINE('',#6137,#683);
#325=LINE('',#6141,#684);
#326=LINE('',#6142,#685);
#327=LINE('',#6145,#686);
#328=LINE('',#6146,#687);
#329=LINE('',#6147,#688);
#330=LINE('',#6148,#689);
#331=LINE('',#6149,#690);
#332=LINE('',#6150,#691);
#333=LINE('',#6154,#692);
#334=LINE('',#6156,#693);
#335=LINE('',#6158,#694);
#336=LINE('',#6160,#695);
#337=LINE('',#6162,#696);
#338=LINE('',#6163,#697);
#339=LINE('',#6164,#698);
#340=LINE('',#6168,#699);
#341=LINE('',#6169,#700);
#342=LINE('',#6170,#701);
#343=LINE('',#6172,#702);
#344=LINE('',#6174,#703);
#345=LINE('',#6176,#704);
#346=LINE('',#6177,#705);
#347=LINE('',#6179,#706);
#348=LINE('',#6181,#707);
#349=LINE('',#6182,#708);
#350=LINE('',#6184,#709);
#351=LINE('',#6186,#710);
#352=LINE('',#6187,#711);
#353=LINE('',#6191,#712);
#354=LINE('',#6193,#713);
#355=LINE('',#6195,#714);
#356=LINE('',#6197,#715);
#357=LINE('',#6199,#716);
#358=LINE('',#6201,#717);
#359=LINE('',#6203,#718);
#360=LINE('',#6207,#719);
#361=LINE('',#6208,#720);
#362=LINE('',#6210,#721);
#363=LINE('',#6212,#722);
#364=LINE('',#6216,#723);
#365=LINE('',#6218,#724);
#366=LINE('',#6219,#725);
#367=LINE('',#6220,#726);
#368=LINE('',#6222,#727);
#369=LINE('',#6224,#728);
#370=LINE('',#6226,#729);
#371=LINE('',#6229,#730);
#372=LINE('',#6230,#731);
#373=LINE('',#6232,#732);
#374=LINE('',#6234,#733);
#375=LINE('',#6236,#734);
#376=LINE('',#6239,#735);
#377=LINE('',#6240,#736);
#378=LINE('',#6244,#737);
#379=LINE('',#6245,#738);
#380=LINE('',#6252,#739);
#381=LINE('',#6253,#740);
#382=LINE('',#6255,#741);
#383=LINE('',#6256,#742);
#384=LINE('',#6259,#743);
#385=LINE('',#6261,#744);
#386=LINE('',#6263,#745);
#387=LINE('',#6265,#746);
#388=LINE('',#6266,#747);
#389=LINE('',#6268,#748);
#390=LINE('',#6269,#749);
#391=LINE('',#6271,#750);
#392=LINE('',#6273,#751);
#393=LINE('',#6285,#752);
#394=LINE('',#6291,#753);
#395=LINE('',#6297,#754);
#396=LINE('',#6315,#755);
#397=LINE('',#6320,#756);
#398=LINE('',#6322,#757);
#399=LINE('',#6324,#758);
#400=LINE('',#6326,#759);
#401=LINE('',#6328,#760);
#402=LINE('',#6329,#761);
#403=LINE('',#6333,#762);
#404=LINE('',#6335,#763);
#405=LINE('',#6336,#764);
#406=LINE('',#6339,#765);
#407=LINE('',#6340,#766);
#408=LINE('',#6343,#767);
#409=LINE('',#6344,#768);
#410=LINE('',#6347,#769);
#411=LINE('',#6348,#770);
#412=LINE('',#6351,#771);
#413=LINE('',#6352,#772);
#414=LINE('',#6354,#773);
#415=LINE('',#6359,#774);
#416=LINE('',#6361,#775);
#417=LINE('',#6363,#776);
#418=LINE('',#6365,#777);
#419=LINE('',#6367,#778);
#420=LINE('',#6368,#779);
#421=LINE('',#6371,#780);
#422=LINE('',#6372,#781);
#423=LINE('',#6375,#782);
#424=LINE('',#6376,#783);
#425=LINE('',#6379,#784);
#426=LINE('',#6380,#785);
#427=LINE('',#6383,#786);
#428=LINE('',#6384,#787);
#429=LINE('',#6387,#788);
#430=LINE('',#6388,#789);
#431=LINE('',#6391,#790);
#432=LINE('',#6392,#791);
#433=LINE('',#6394,#792);
#434=LINE('',#6395,#793);
#435=LINE('',#6397,#794);
#436=LINE('',#6399,#795);
#437=LINE('',#6401,#796);
#438=LINE('',#6403,#797);
#439=LINE('',#6413,#798);
#440=LINE('',#6416,#799);
#441=LINE('',#6422,#800);
#442=LINE('',#6425,#801);
#443=LINE('',#6431,#802);
#444=LINE('',#6434,#803);
#445=LINE('',#6439,#804);
#446=LINE('',#6445,#805);
#447=LINE('',#6451,#806);
#448=LINE('',#6459,#807);
#449=LINE('',#6464,#808);
#450=LINE('',#6470,#809);
#451=LINE('',#6477,#810);
#452=LINE('',#6483,#811);
#453=LINE('',#6489,#812);
#454=LINE('',#6493,#813);
#455=LINE('',#6495,#814);
#456=LINE('',#6499,#815);
#457=LINE('',#6501,#816);
#458=LINE('',#6503,#817);
#459=LINE('',#6505,#818);
#460=LINE('',#6507,#819);
#461=LINE('',#6509,#820);
#462=LINE('',#6511,#821);
#463=LINE('',#6513,#822);
#464=LINE('',#6515,#823);
#465=LINE('',#6517,#824);
#466=LINE('',#6519,#825);
#467=LINE('',#6521,#826);
#468=LINE('',#6523,#827);
#469=LINE('',#6525,#828);
#470=LINE('',#6527,#829);
#471=LINE('',#6529,#830);
#472=LINE('',#6531,#831);
#473=LINE('',#6533,#832);
#474=LINE('',#6535,#833);
#475=LINE('',#6536,#834);
#476=LINE('',#6540,#835);
#477=LINE('',#6542,#836);
#478=LINE('',#6544,#837);
#479=LINE('',#6546,#838);
#480=LINE('',#6548,#839);
#481=LINE('',#6550,#840);
#482=LINE('',#6552,#841);
#483=LINE('',#6554,#842);
#484=LINE('',#6556,#843);
#485=LINE('',#6558,#844);
#486=LINE('',#6560,#845);
#487=LINE('',#6562,#846);
#488=LINE('',#6564,#847);
#489=LINE('',#6566,#848);
#490=LINE('',#6568,#849);
#491=LINE('',#6570,#850);
#492=LINE('',#6572,#851);
#493=LINE('',#6574,#852);
#494=LINE('',#6576,#853);
#495=LINE('',#6577,#854);
#496=LINE('',#6580,#855);
#497=LINE('',#6583,#856);
#498=LINE('',#6586,#857);
#499=LINE('',#6589,#858);
#500=LINE('',#6592,#859);
#501=LINE('',#6595,#860);
#502=LINE('',#6598,#861);
#503=LINE('',#6601,#862);
#504=LINE('',#6603,#863);
#505=LINE('',#6605,#864);
#506=LINE('',#6609,#865);
#507=LINE('',#6611,#866);
#508=LINE('',#6623,#867);
#509=LINE('',#6624,#868);
#510=LINE('',#6626,#869);
#511=LINE('',#6627,#870);
#512=LINE('',#6635,#871);
#513=LINE('',#6641,#872);
#514=LINE('',#6648,#873);
#515=LINE('',#6651,#874);
#516=LINE('',#6654,#875);
#517=LINE('',#6657,#876);
#518=LINE('',#6660,#877);
#519=LINE('',#6663,#878);
#520=LINE('',#6665,#879);
#521=LINE('',#6667,#880);
#522=LINE('',#6674,#881);
#523=LINE('',#6680,#882);
#524=LINE('',#6688,#883);
#525=LINE('',#6696,#884);
#526=LINE('',#6701,#885);
#527=LINE('',#6704,#886);
#528=LINE('',#6710,#887);
#529=LINE('',#6715,#888);
#530=LINE('',#6718,#889);
#531=LINE('',#6753,#890);
#532=LINE('',#6757,#891);
#533=LINE('',#6760,#892);
#534=LINE('',#6765,#893);
#535=LINE('',#6772,#894);
#536=LINE('',#6775,#895);
#537=LINE('',#6780,#896);
#538=LINE('',#6841,#897);
#539=LINE('',#6899,#898);
#540=LINE('',#6970,#899);
#541=LINE('',#7039,#900);
#542=LINE('',#7043,#901);
#543=LINE('',#7047,#902);
#544=LINE('',#7049,#903);
#545=LINE('',#7050,#904);
#546=LINE('',#7052,#905);
#547=LINE('',#7053,#906);
#548=LINE('',#7055,#907);
#549=LINE('',#7057,#908);
#550=LINE('',#7058,#909);
#551=LINE('',#7062,#910);
#552=LINE('',#7063,#911);
#553=LINE('',#7065,#912);
#554=LINE('',#7067,#913);
#555=LINE('',#7068,#914);
#556=LINE('',#7069,#915);
#557=LINE('',#7073,#916);
#558=LINE('',#7078,#917);
#559=LINE('',#7080,#918);
#560=LINE('',#7084,#919);
#561=LINE('',#7087,#920);
#562=LINE('',#7089,#921);
#563=LINE('',#7093,#922);
#564=LINE('',#7097,#923);
#565=LINE('',#7099,#924);
#566=LINE('',#7101,#925);
#567=LINE('',#7103,#926);
#568=LINE('',#7104,#927);
#569=LINE('',#7109,#928);
#570=LINE('',#7111,#929);
#571=LINE('',#7113,#930);
#572=LINE('',#7115,#931);
#573=LINE('',#7117,#932);
#574=LINE('',#7119,#933);
#575=LINE('',#7121,#934);
#576=LINE('',#7125,#935);
#577=LINE('',#7128,#936);
#578=LINE('',#7130,#937);
#579=LINE('',#7133,#938);
#580=LINE('',#7137,#939);
#581=LINE('',#7138,#940);
#582=LINE('',#7139,#941);
#583=LINE('',#7143,#942);
#584=LINE('',#7144,#943);
#585=LINE('',#7147,#944);
#586=LINE('',#7148,#945);
#587=LINE('',#7153,#946);
#588=LINE('',#7155,#947);
#589=LINE('',#7157,#948);
#590=LINE('',#7158,#949);
#591=LINE('',#7162,#950);
#592=LINE('',#7164,#951);
#593=LINE('',#7168,#952);
#594=LINE('',#7170,#953);
#595=LINE('',#7172,#954);
#596=LINE('',#7179,#955);
#597=LINE('',#7181,#956);
#598=LINE('',#7182,#957);
#599=LINE('',#7191,#958);
#600=LINE('',#7193,#959);
#601=LINE('',#7195,#960);
#602=LINE('',#7196,#961);
#603=LINE('',#7614,#962);
#604=LINE('',#7620,#963);
#605=LINE('',#7627,#964);
#606=LINE('',#7630,#965);
#607=LINE('',#7633,#966);
#608=LINE('',#7636,#967);
#609=LINE('',#7639,#968);
#610=LINE('',#7642,#969);
#611=LINE('',#7644,#970);
#612=LINE('',#7646,#971);
#613=LINE('',#7655,#972);
#614=LINE('',#7663,#973);
#615=LINE('',#7669,#974);
#616=LINE('',#7675,#975);
#617=LINE('',#7680,#976);
#618=LINE('',#7683,#977);
#619=LINE('',#7688,#978);
#620=LINE('',#7691,#979);
#621=LINE('',#7696,#980);
#622=LINE('',#7698,#981);
#623=LINE('',#7700,#982);
#624=LINE('',#7702,#983);
#625=LINE('',#7704,#984);
#626=LINE('',#7706,#985);
#627=LINE('',#7708,#986);
#628=LINE('',#7710,#987);
#629=LINE('',#7711,#988);
#630=LINE('',#7715,#989);
#631=LINE('',#7717,#990);
#632=LINE('',#7719,#991);
#633=LINE('',#7721,#992);
#634=LINE('',#7723,#993);
#635=LINE('',#7725,#994);
#636=LINE('',#7727,#995);
#637=LINE('',#7729,#996);
#638=LINE('',#7730,#997);
#639=LINE('',#7732,#998);
#640=LINE('',#7733,#999);
#641=LINE('',#7735,#1000);
#642=LINE('',#7737,#1001);
#643=LINE('',#7739,#1002);
#644=LINE('',#7741,#1003);
#645=LINE('',#7743,#1004);
#646=LINE('',#7745,#1005);
#647=LINE('',#7747,#1006);
#648=VECTOR('',#4740,5.00000000000003);
#649=VECTOR('',#4753,5.00000000000003);
#650=VECTOR('',#4758,1000.);
#651=VECTOR('',#4761,1000.);
#652=VECTOR('',#4766,5.00000000000002);
#653=VECTOR('',#4773,5.00000000000002);
#654=VECTOR('',#4780,1000.);
#655=VECTOR('',#4783,1000.);
#656=VECTOR('',#4788,1000.);
#657=VECTOR('',#4791,1000.);
#658=VECTOR('',#4796,1000.);
#659=VECTOR('',#4799,1000.);
#660=VECTOR('',#4804,1000.);
#661=VECTOR('',#4807,1000.);
#662=VECTOR('',#4812,1000.);
#663=VECTOR('',#4813,1000.);
#664=VECTOR('',#4816,1000.);
#665=VECTOR('',#4819,1000.);
#666=VECTOR('',#4822,1000.);
#667=VECTOR('',#4823,1000.);
#668=VECTOR('',#4824,1000.);
#669=VECTOR('',#4825,1000.);
#670=VECTOR('',#4826,1000.);
#671=VECTOR('',#4829,1000.);
#672=VECTOR('',#4830,1000.);
#673=VECTOR('',#4831,1000.);
#674=VECTOR('',#4832,1000.);
#675=VECTOR('',#4833,1000.);
#676=VECTOR('',#4834,1000.);
#677=VECTOR('',#4835,1000.);
#678=VECTOR('',#4836,1000.);
#679=VECTOR('',#4837,1000.);
#680=VECTOR('',#4838,1000.);
#681=VECTOR('',#4839,1000.);
#682=VECTOR('',#4840,1000.);
#683=VECTOR('',#4841,1000.);
#684=VECTOR('',#4844,1000.);
#685=VECTOR('',#4845,1000.);
#686=VECTOR('',#4848,1000.);
#687=VECTOR('',#4849,1000.);
#688=VECTOR('',#4850,1000.);
#689=VECTOR('',#4851,1000.);
#690=VECTOR('',#4852,1000.);
#691=VECTOR('',#4853,1000.);
#692=VECTOR('',#4856,1000.);
#693=VECTOR('',#4857,1000.);
#694=VECTOR('',#4858,1000.);
#695=VECTOR('',#4859,1000.);
#696=VECTOR('',#4860,1000.);
#697=VECTOR('',#4861,1000.);
#698=VECTOR('',#4862,1000.);
#699=VECTOR('',#4865,1000.);
#700=VECTOR('',#4866,1000.);
#701=VECTOR('',#4867,1000.);
#702=VECTOR('',#4870,1000.);
#703=VECTOR('',#4871,1000.);
#704=VECTOR('',#4872,1000.);
#705=VECTOR('',#4873,1000.);
#706=VECTOR('',#4874,1000.);
#707=VECTOR('',#4875,1000.);
#708=VECTOR('',#4876,1000.);
#709=VECTOR('',#4877,1000.);
#710=VECTOR('',#4878,1000.);
#711=VECTOR('',#4879,1000.);
#712=VECTOR('',#4884,1000.);
#713=VECTOR('',#4887,1000.);
#714=VECTOR('',#4890,1000.);
#715=VECTOR('',#4893,1000.);
#716=VECTOR('',#4896,1000.);
#717=VECTOR('',#4899,1000.);
#718=VECTOR('',#4900,1000.);
#719=VECTOR('',#4903,1000.);
#720=VECTOR('',#4904,1000.);
#721=VECTOR('',#4905,1000.);
#722=VECTOR('',#4906,1000.);
#723=VECTOR('',#4909,1000.);
#724=VECTOR('',#4910,1000.);
#725=VECTOR('',#4911,1000.);
#726=VECTOR('',#4912,1000.);
#727=VECTOR('',#4915,1000.);
#728=VECTOR('',#4918,1000.);
#729=VECTOR('',#4921,1000.);
#730=VECTOR('',#4926,1000.);
#731=VECTOR('',#4927,1000.);
#732=VECTOR('',#4930,1000.);
#733=VECTOR('',#4933,1000.);
#734=VECTOR('',#4936,1000.);
#735=VECTOR('',#4941,1000.);
#736=VECTOR('',#4942,1000.);
#737=VECTOR('',#4949,1000.);
#738=VECTOR('',#4950,1000.);
#739=VECTOR('',#4961,1000.);
#740=VECTOR('',#4962,1000.);
#741=VECTOR('',#4963,1000.);
#742=VECTOR('',#4964,1000.);
#743=VECTOR('',#4967,1000.);
#744=VECTOR('',#4968,1000.);
#745=VECTOR('',#4969,1000.);
#746=VECTOR('',#4970,1000.);
#747=VECTOR('',#4971,1000.);
#748=VECTOR('',#4974,1000.);
#749=VECTOR('',#4975,1000.);
#750=VECTOR('',#4978,1000.);
#751=VECTOR('',#4981,1000.);
#752=VECTOR('',#5000,6.);
#753=VECTOR('',#5007,5.);
#754=VECTOR('',#5014,10.);
#755=VECTOR('',#5033,14.);
#756=VECTOR('',#5038,1000.);
#757=VECTOR('',#5039,1000.);
#758=VECTOR('',#5040,1000.);
#759=VECTOR('',#5041,1000.);
#760=VECTOR('',#5042,1000.);
#761=VECTOR('',#5043,1000.);
#762=VECTOR('',#5048,1000.);
#763=VECTOR('',#5049,1000.);
#764=VECTOR('',#5050,1000.);
#765=VECTOR('',#5053,1000.);
#766=VECTOR('',#5054,1000.);
#767=VECTOR('',#5057,1000.);
#768=VECTOR('',#5058,1000.);
#769=VECTOR('',#5061,1000.);
#770=VECTOR('',#5062,1000.);
#771=VECTOR('',#5065,1000.);
#772=VECTOR('',#5066,1000.);
#773=VECTOR('',#5069,1000.);
#774=VECTOR('',#5074,1000.);
#775=VECTOR('',#5075,1000.);
#776=VECTOR('',#5076,1000.);
#777=VECTOR('',#5077,1000.);
#778=VECTOR('',#5078,1000.);
#779=VECTOR('',#5079,1000.);
#780=VECTOR('',#5082,1000.);
#781=VECTOR('',#5083,1000.);
#782=VECTOR('',#5086,1000.);
#783=VECTOR('',#5087,1000.);
#784=VECTOR('',#5090,1000.);
#785=VECTOR('',#5091,1000.);
#786=VECTOR('',#5094,1000.);
#787=VECTOR('',#5095,1000.);
#788=VECTOR('',#5098,1000.);
#789=VECTOR('',#5099,1000.);
#790=VECTOR('',#5102,1000.);
#791=VECTOR('',#5103,1000.);
#792=VECTOR('',#5106,1000.);
#793=VECTOR('',#5107,1000.);
#794=VECTOR('',#5110,1000.);
#795=VECTOR('',#5113,1000.);
#796=VECTOR('',#5116,1000.);
#797=VECTOR('',#5119,1000.);
#798=VECTOR('',#5132,1000.);
#799=VECTOR('',#5135,1000.);
#800=VECTOR('',#5140,1000.);
#801=VECTOR('',#5143,1000.);
#802=VECTOR('',#5148,1000.);
#803=VECTOR('',#5151,1000.);
#804=VECTOR('',#5156,6.);
#805=VECTOR('',#5163,10.);
#806=VECTOR('',#5170,10.);
#807=VECTOR('',#5181,5.);
#808=VECTOR('',#5186,5.);
#809=VECTOR('',#5193,5.);
#810=VECTOR('',#5202,5.);
#811=VECTOR('',#5209,5.);
#812=VECTOR('',#5216,5.);
#813=VECTOR('',#5223,1000.);
#814=VECTOR('',#5226,1000.);
#815=VECTOR('',#5229,1000.);
#816=VECTOR('',#5230,1000.);
#817=VECTOR('',#5231,1000.);
#818=VECTOR('',#5232,1000.);
#819=VECTOR('',#5233,1000.);
#820=VECTOR('',#5234,1000.);
#821=VECTOR('',#5235,1000.);
#822=VECTOR('',#5236,1000.);
#823=VECTOR('',#5237,1000.);
#824=VECTOR('',#5238,1000.);
#825=VECTOR('',#5239,1000.);
#826=VECTOR('',#5240,1000.);
#827=VECTOR('',#5241,1000.);
#828=VECTOR('',#5242,1000.);
#829=VECTOR('',#5243,1000.);
#830=VECTOR('',#5244,1000.);
#831=VECTOR('',#5245,1000.);
#832=VECTOR('',#5246,1000.);
#833=VECTOR('',#5247,1000.);
#834=VECTOR('',#5248,1000.);
#835=VECTOR('',#5251,1000.);
#836=VECTOR('',#5252,1000.);
#837=VECTOR('',#5253,1000.);
#838=VECTOR('',#5254,1000.);
#839=VECTOR('',#5255,1000.);
#840=VECTOR('',#5256,1000.);
#841=VECTOR('',#5257,1000.);
#842=VECTOR('',#5258,1000.);
#843=VECTOR('',#5259,1000.);
#844=VECTOR('',#5260,1000.);
#845=VECTOR('',#5261,1000.);
#846=VECTOR('',#5262,1000.);
#847=VECTOR('',#5263,1000.);
#848=VECTOR('',#5264,1000.);
#849=VECTOR('',#5265,1000.);
#850=VECTOR('',#5266,1000.);
#851=VECTOR('',#5267,1000.);
#852=VECTOR('',#5268,1000.);
#853=VECTOR('',#5269,1000.);
#854=VECTOR('',#5270,1000.);
#855=VECTOR('',#5275,1000.);
#856=VECTOR('',#5280,1000.);
#857=VECTOR('',#5285,1000.);
#858=VECTOR('',#5290,1000.);
#859=VECTOR('',#5295,1000.);
#860=VECTOR('',#5300,1000.);
#861=VECTOR('',#5305,1000.);
#862=VECTOR('',#5310,1000.);
#863=VECTOR('',#5313,1000.);
#864=VECTOR('',#5316,1000.);
#865=VECTOR('',#5323,1000.);
#866=VECTOR('',#5326,1000.);
#867=VECTOR('',#5349,1000.);
#868=VECTOR('',#5350,1000.);
#869=VECTOR('',#5353,1000.);
#870=VECTOR('',#5354,1000.);
#871=VECTOR('',#5365,5.);
#872=VECTOR('',#5372,5.);
#873=VECTOR('',#5379,1000.);
#874=VECTOR('',#5382,1000.);
#875=VECTOR('',#5385,1000.);
#876=VECTOR('',#5388,1000.);
#877=VECTOR('',#5391,1000.);
#878=VECTOR('',#5394,1000.);
#879=VECTOR('',#5397,1000.);
#880=VECTOR('',#5400,1000.);
#881=VECTOR('',#5409,3.99999999999998);
#882=VECTOR('',#5416,3.99999999999998);
#883=VECTOR('',#5425,5.);
#884=VECTOR('',#5434,5.);
#885=VECTOR('',#5441,5.);
#886=VECTOR('',#5444,5.);
#887=VECTOR('',#5451,5.);
#888=VECTOR('',#5458,5.);
#889=VECTOR('',#5461,5.);
#890=VECTOR('',#5500,5.);
#891=VECTOR('',#5505,1000.);
#892=VECTOR('',#5508,1000.);
#893=VECTOR('',#5513,5.);
#894=VECTOR('',#5520,1000.);
#895=VECTOR('',#5523,1000.);
#896=VECTOR('',#5528,10.);
#897=VECTOR('',#5531,1000.);
#898=VECTOR('',#5532,10.);
#899=VECTOR('',#5535,1000.);
#900=VECTOR('',#5540,1000.);
#901=VECTOR('',#5543,1000.);
#902=VECTOR('',#5546,1000.);
#903=VECTOR('',#5547,1000.);
#904=VECTOR('',#5548,1000.);
#905=VECTOR('',#5551,1000.);
#906=VECTOR('',#5552,1000.);
#907=VECTOR('',#5553,1000.);
#908=VECTOR('',#5554,1000.);
#909=VECTOR('',#5555,1000.);
#910=VECTOR('',#5558,1000.);
#911=VECTOR('',#5559,1000.);
#912=VECTOR('',#5560,1000.);
#913=VECTOR('',#5561,1000.);
#914=VECTOR('',#5562,1000.);
#915=VECTOR('',#5563,1000.);
#916=VECTOR('',#5566,1000.);
#917=VECTOR('',#5573,1000.);
#918=VECTOR('',#5574,1000.);
#919=VECTOR('',#5577,1000.);
#920=VECTOR('',#5580,1000.);
#921=VECTOR('',#5581,1000.);
#922=VECTOR('',#5584,1000.);
#923=VECTOR('',#5587,1000.);
#924=VECTOR('',#5588,1000.);
#925=VECTOR('',#5589,1000.);
#926=VECTOR('',#5590,1000.);
#927=VECTOR('',#5591,1000.);
#928=VECTOR('',#5596,1000.);
#929=VECTOR('',#5597,1000.);
#930=VECTOR('',#5598,1000.);
#931=VECTOR('',#5599,1000.);
#932=VECTOR('',#5600,1000.);
#933=VECTOR('',#5601,1000.);
#934=VECTOR('',#5602,1000.);
#935=VECTOR('',#5605,1000.);
#936=VECTOR('',#5608,1000.);
#937=VECTOR('',#5609,1000.);
#938=VECTOR('',#5612,1000.);
#939=VECTOR('',#5615,1000.);
#940=VECTOR('',#5616,1000.);
#941=VECTOR('',#5617,1000.);
#942=VECTOR('',#5624,1000.);
#943=VECTOR('',#5625,1000.);
#944=VECTOR('',#5630,1000.);
#945=VECTOR('',#5631,1000.);
#946=VECTOR('',#5636,1000.);
#947=VECTOR('',#5637,1000.);
#948=VECTOR('',#5638,1000.);
#949=VECTOR('',#5639,1000.);
#950=VECTOR('',#5644,1000.);
#951=VECTOR('',#5645,1000.);
#952=VECTOR('',#5648,1000.);
#953=VECTOR('',#5649,1000.);
#954=VECTOR('',#5650,1000.);
#955=VECTOR('',#5657,1000.);
#956=VECTOR('',#5658,1000.);
#957=VECTOR('',#5659,1000.);
#958=VECTOR('',#5672,1000.);
#959=VECTOR('',#5673,1000.);
#960=VECTOR('',#5674,1000.);
#961=VECTOR('',#5675,1000.);
#962=VECTOR('',#5826,5.);
#963=VECTOR('',#5833,5.);
#964=VECTOR('',#5840,1000.);
#965=VECTOR('',#5843,1000.);
#966=VECTOR('',#5846,1000.);
#967=VECTOR('',#5849,1000.);
#968=VECTOR('',#5852,1000.);
#969=VECTOR('',#5855,1000.);
#970=VECTOR('',#5858,1000.);
#971=VECTOR('',#5861,1000.);
#972=VECTOR('',#5872,5.);
#973=VECTOR('',#5881,5.);
#974=VECTOR('',#5888,3.99999999999998);
#975=VECTOR('',#5895,3.99999999999998);
#976=VECTOR('',#5902,5.);
#977=VECTOR('',#5905,5.);
#978=VECTOR('',#5912,5.);
#979=VECTOR('',#5915,5.);
#980=VECTOR('',#5920,1000.);
#981=VECTOR('',#5921,1000.);
#982=VECTOR('',#5922,1000.);
#983=VECTOR('',#5923,1000.);
#984=VECTOR('',#5924,1000.);
#985=VECTOR('',#5925,1000.);
#986=VECTOR('',#5926,1000.);
#987=VECTOR('',#5927,1000.);
#988=VECTOR('',#5928,1000.);
#989=VECTOR('',#5931,1000.);
#990=VECTOR('',#5932,1000.);
#991=VECTOR('',#5933,1000.);
#992=VECTOR('',#5934,1000.);
#993=VECTOR('',#5935,1000.);
#994=VECTOR('',#5936,1000.);
#995=VECTOR('',#5937,1000.);
#996=VECTOR('',#5938,1000.);
#997=VECTOR('',#5939,1000.);
#998=VECTOR('',#5942,1000.);
#999=VECTOR('',#5943,1000.);
#1000=VECTOR('',#5946,1000.);
#1001=VECTOR('',#5949,1000.);
#1002=VECTOR('',#5952,1000.);
#1003=VECTOR('',#5955,1000.);
#1004=VECTOR('',#5958,1000.);
#1005=VECTOR('',#5961,1000.);
#1006=VECTOR('',#5964,1000.);
#1007=CYLINDRICAL_SURFACE('',#4261,5.00000000000003);
#1008=CYLINDRICAL_SURFACE('',#4267,5.00000000000003);
#1009=CYLINDRICAL_SURFACE('',#4269,5.);
#1010=CYLINDRICAL_SURFACE('',#4272,5.00000000000002);
#1011=CYLINDRICAL_SURFACE('',#4275,5.00000000000002);
#1012=CYLINDRICAL_SURFACE('',#4278,23.5);
#1013=CYLINDRICAL_SURFACE('',#4281,22.);
#1014=CYLINDRICAL_SURFACE('',#4284,15.);
#1015=CYLINDRICAL_SURFACE('',#4287,55.);
#1016=CYLINDRICAL_SURFACE('',#4290,34.);
#1017=CYLINDRICAL_SURFACE('',#4292,34.);
#1018=CYLINDRICAL_SURFACE('',#4312,10.);
#1019=CYLINDRICAL_SURFACE('',#4316,10.);
#1020=CYLINDRICAL_SURFACE('',#4339,6.);
#1021=CYLINDRICAL_SURFACE('',#4342,5.);
#1022=CYLINDRICAL_SURFACE('',#4345,10.);
#1023=CYLINDRICAL_SURFACE('',#4354,14.);
#1024=CYLINDRICAL_SURFACE('',#4382,1.5);
#1025=CYLINDRICAL_SURFACE('',#4385,2.5);
#1026=CYLINDRICAL_SURFACE('',#4388,2.5);
#1027=CYLINDRICAL_SURFACE('',#4391,6.);
#1028=CYLINDRICAL_SURFACE('',#4394,10.);
#1029=CYLINDRICAL_SURFACE('',#4397,10.);
#1030=CYLINDRICAL_SURFACE('',#4402,5.);
#1031=CYLINDRICAL_SURFACE('',#4404,5.);
#1032=CYLINDRICAL_SURFACE('',#4407,5.);
#1033=CYLINDRICAL_SURFACE('',#4411,5.);
#1034=CYLINDRICAL_SURFACE('',#4414,5.);
#1035=CYLINDRICAL_SURFACE('',#4417,5.);
#1036=CYLINDRICAL_SURFACE('',#4420,2.5);
#1037=CYLINDRICAL_SURFACE('',#4449,10.);
#1038=CYLINDRICAL_SURFACE('',#4450,10.);
#1039=CYLINDRICAL_SURFACE('',#4451,10.);
#1040=CYLINDRICAL_SURFACE('',#4452,10.);
#1041=CYLINDRICAL_SURFACE('',#4462,5.);
#1042=CYLINDRICAL_SURFACE('',#4465,5.);
#1043=CYLINDRICAL_SURFACE('',#4468,10.);
#1044=CYLINDRICAL_SURFACE('',#4476,10.);
#1045=CYLINDRICAL_SURFACE('',#4493,5.);
#1046=CYLINDRICAL_SURFACE('',#4495,5.);
#1047=CYLINDRICAL_SURFACE('',#4497,5.);
#1048=CYLINDRICAL_SURFACE('',#4500,5.);
#1049=CYLINDRICAL_SURFACE('',#4502,5.);
#1050=CYLINDRICAL_SURFACE('',#4520,5.);
#1051=CYLINDRICAL_SURFACE('',#4523,10.);
#1052=CYLINDRICAL_SURFACE('',#4525,5.);
#1053=CYLINDRICAL_SURFACE('',#4528,10.);
#1054=CYLINDRICAL_SURFACE('',#4531,10.);
#1055=CYLINDRICAL_SURFACE('',#4541,20.);
#1056=CYLINDRICAL_SURFACE('',#4555,10.);
#1057=CYLINDRICAL_SURFACE('',#4568,10.);
#1058=CYLINDRICAL_SURFACE('',#4575,7.);
#1059=CYLINDRICAL_SURFACE('',#4578,7.);
#1060=CYLINDRICAL_SURFACE('',#4581,2.);
#1061=CYLINDRICAL_SURFACE('',#4583,2.);
#1062=CYLINDRICAL_SURFACE('',#4589,2.);
#1063=CYLINDRICAL_SURFACE('',#4591,2.);
#1064=CYLINDRICAL_SURFACE('',#4594,2.);
#1065=CYLINDRICAL_SURFACE('',#4600,2.);
#1066=CYLINDRICAL_SURFACE('',#4601,2.);
#1067=CYLINDRICAL_SURFACE('',#4605,2.);
#1068=CYLINDRICAL_SURFACE('',#4609,2.);
#1069=CYLINDRICAL_SURFACE('',#4613,2.);
#1070=CYLINDRICAL_SURFACE('',#4615,2.);
#1071=CYLINDRICAL_SURFACE('',#4621,2.);
#1072=CYLINDRICAL_SURFACE('',#4623,2.);
#1073=CYLINDRICAL_SURFACE('',#4625,2.);
#1074=CYLINDRICAL_SURFACE('',#4632,2.);
#1075=CYLINDRICAL_SURFACE('',#4633,2.);
#1076=CYLINDRICAL_SURFACE('',#4640,2.);
#1077=CYLINDRICAL_SURFACE('',#4641,2.);
#1078=CYLINDRICAL_SURFACE('',#4647,5.);
#1079=CYLINDRICAL_SURFACE('',#4650,5.);
#1080=CYLINDRICAL_SURFACE('',#4653,10.);
#1081=CYLINDRICAL_SURFACE('',#4661,10.);
#1082=CYLINDRICAL_SURFACE('',#4678,5.);
#1083=CYLINDRICAL_SURFACE('',#4680,5.);
#1084=CYLINDRICAL_SURFACE('',#4682,5.);
#1085=CYLINDRICAL_SURFACE('',#4684,5.);
#1086=FACE_OUTER_BOUND('',#1329,.T.);
#1087=FACE_OUTER_BOUND('',#1330,.T.);
#1088=FACE_OUTER_BOUND('',#1331,.T.);
#1089=FACE_OUTER_BOUND('',#1332,.T.);
#1090=FACE_OUTER_BOUND('',#1333,.T.);
#1091=FACE_OUTER_BOUND('',#1334,.T.);
#1092=FACE_OUTER_BOUND('',#1335,.T.);
#1093=FACE_OUTER_BOUND('',#1336,.T.);
#1094=FACE_OUTER_BOUND('',#1337,.T.);
#1095=FACE_OUTER_BOUND('',#1338,.T.);
#1096=FACE_OUTER_BOUND('',#1339,.T.);
#1097=FACE_OUTER_BOUND('',#1340,.T.);
#1098=FACE_OUTER_BOUND('',#1341,.T.);
#1099=FACE_OUTER_BOUND('',#1342,.T.);
#1100=FACE_OUTER_BOUND('',#1343,.T.);
#1101=FACE_OUTER_BOUND('',#1348,.T.);
#1102=FACE_OUTER_BOUND('',#1349,.T.);
#1103=FACE_OUTER_BOUND('',#1350,.T.);
#1104=FACE_OUTER_BOUND('',#1351,.T.);
#1105=FACE_OUTER_BOUND('',#1353,.T.);
#1106=FACE_OUTER_BOUND('',#1354,.T.);
#1107=FACE_OUTER_BOUND('',#1355,.T.);
#1108=FACE_OUTER_BOUND('',#1356,.T.);
#1109=FACE_OUTER_BOUND('',#1357,.T.);
#1110=FACE_OUTER_BOUND('',#1358,.T.);
#1111=FACE_OUTER_BOUND('',#1361,.T.);
#1112=FACE_OUTER_BOUND('',#1362,.T.);
#1113=FACE_OUTER_BOUND('',#1363,.T.);
#1114=FACE_OUTER_BOUND('',#1364,.T.);
#1115=FACE_OUTER_BOUND('',#1365,.T.);
#1116=FACE_OUTER_BOUND('',#1366,.T.);
#1117=FACE_OUTER_BOUND('',#1367,.T.);
#1118=FACE_OUTER_BOUND('',#1368,.T.);
#1119=FACE_OUTER_BOUND('',#1369,.T.);
#1120=FACE_OUTER_BOUND('',#1370,.T.);
#1121=FACE_OUTER_BOUND('',#1371,.T.);
#1122=FACE_OUTER_BOUND('',#1372,.T.);
#1123=FACE_OUTER_BOUND('',#1373,.T.);
#1124=FACE_OUTER_BOUND('',#1374,.T.);
#1125=FACE_OUTER_BOUND('',#1375,.T.);
#1126=FACE_OUTER_BOUND('',#1376,.T.);
#1127=FACE_OUTER_BOUND('',#1377,.T.);
#1128=FACE_OUTER_BOUND('',#1378,.T.);
#1129=FACE_OUTER_BOUND('',#1379,.T.);
#1130=FACE_OUTER_BOUND('',#1380,.T.);
#1131=FACE_OUTER_BOUND('',#1381,.T.);
#1132=FACE_OUTER_BOUND('',#1382,.T.);
#1133=FACE_OUTER_BOUND('',#1383,.T.);
#1134=FACE_OUTER_BOUND('',#1384,.T.);
#1135=FACE_OUTER_BOUND('',#1385,.T.);
#1136=FACE_OUTER_BOUND('',#1386,.T.);
#1137=FACE_OUTER_BOUND('',#1387,.T.);
#1138=FACE_OUTER_BOUND('',#1388,.T.);
#1139=FACE_OUTER_BOUND('',#1389,.T.);
#1140=FACE_OUTER_BOUND('',#1390,.T.);
#1141=FACE_OUTER_BOUND('',#1391,.T.);
#1142=FACE_OUTER_BOUND('',#1392,.T.);
#1143=FACE_OUTER_BOUND('',#1394,.T.);
#1144=FACE_OUTER_BOUND('',#1396,.T.);
#1145=FACE_OUTER_BOUND('',#1397,.T.);
#1146=FACE_OUTER_BOUND('',#1398,.T.);
#1147=FACE_OUTER_BOUND('',#1399,.T.);
#1148=FACE_OUTER_BOUND('',#1400,.T.);
#1149=FACE_OUTER_BOUND('',#1401,.T.);
#1150=FACE_OUTER_BOUND('',#1402,.T.);
#1151=FACE_OUTER_BOUND('',#1403,.T.);
#1152=FACE_OUTER_BOUND('',#1405,.T.);
#1153=FACE_OUTER_BOUND('',#1406,.T.);
#1154=FACE_OUTER_BOUND('',#1407,.T.);
#1155=FACE_OUTER_BOUND('',#1408,.T.);
#1156=FACE_OUTER_BOUND('',#1409,.T.);
#1157=FACE_OUTER_BOUND('',#1410,.T.);
#1158=FACE_OUTER_BOUND('',#1411,.T.);
#1159=FACE_OUTER_BOUND('',#1412,.T.);
#1160=FACE_OUTER_BOUND('',#1413,.T.);
#1161=FACE_OUTER_BOUND('',#1414,.T.);
#1162=FACE_OUTER_BOUND('',#1415,.T.);
#1163=FACE_OUTER_BOUND('',#1416,.T.);
#1164=FACE_OUTER_BOUND('',#1417,.T.);
#1165=FACE_OUTER_BOUND('',#1418,.T.);
#1166=FACE_OUTER_BOUND('',#1420,.T.);
#1167=FACE_OUTER_BOUND('',#1421,.T.);
#1168=FACE_OUTER_BOUND('',#1422,.T.);
#1169=FACE_OUTER_BOUND('',#1423,.T.);
#1170=FACE_OUTER_BOUND('',#1424,.T.);
#1171=FACE_OUTER_BOUND('',#1425,.T.);
#1172=FACE_OUTER_BOUND('',#1426,.T.);
#1173=FACE_OUTER_BOUND('',#1427,.T.);
#1174=FACE_OUTER_BOUND('',#1428,.T.);
#1175=FACE_OUTER_BOUND('',#1429,.T.);
#1176=FACE_OUTER_BOUND('',#1430,.T.);
#1177=FACE_OUTER_BOUND('',#1431,.T.);
#1178=FACE_OUTER_BOUND('',#1432,.T.);
#1179=FACE_OUTER_BOUND('',#1433,.T.);
#1180=FACE_OUTER_BOUND('',#1434,.T.);
#1181=FACE_OUTER_BOUND('',#1435,.T.);
#1182=FACE_OUTER_BOUND('',#1437,.T.);
#1183=FACE_OUTER_BOUND('',#1439,.T.);
#1184=FACE_OUTER_BOUND('',#1441,.T.);
#1185=FACE_OUTER_BOUND('',#1443,.T.);
#1186=FACE_OUTER_BOUND('',#1445,.T.);
#1187=FACE_OUTER_BOUND('',#1447,.T.);
#1188=FACE_OUTER_BOUND('',#1449,.T.);
#1189=FACE_OUTER_BOUND('',#1451,.T.);
#1190=FACE_OUTER_BOUND('',#1453,.T.);
#1191=FACE_OUTER_BOUND('',#1455,.T.);
#1192=FACE_OUTER_BOUND('',#1456,.T.);
#1193=FACE_OUTER_BOUND('',#1458,.T.);
#1194=FACE_OUTER_BOUND('',#1459,.T.);
#1195=FACE_OUTER_BOUND('',#1460,.T.);
#1196=FACE_OUTER_BOUND('',#1461,.T.);
#1197=FACE_OUTER_BOUND('',#1463,.T.);
#1198=FACE_OUTER_BOUND('',#1464,.T.);
#1199=FACE_OUTER_BOUND('',#1465,.T.);
#1200=FACE_OUTER_BOUND('',#1466,.T.);
#1201=FACE_OUTER_BOUND('',#1467,.T.);
#1202=FACE_OUTER_BOUND('',#1468,.T.);
#1203=FACE_OUTER_BOUND('',#1469,.T.);
#1204=FACE_OUTER_BOUND('',#1470,.T.);
#1205=FACE_OUTER_BOUND('',#1471,.T.);
#1206=FACE_OUTER_BOUND('',#1473,.T.);
#1207=FACE_OUTER_BOUND('',#1475,.T.);
#1208=FACE_OUTER_BOUND('',#1476,.T.);
#1209=FACE_OUTER_BOUND('',#1477,.T.);
#1210=FACE_OUTER_BOUND('',#1478,.T.);
#1211=FACE_OUTER_BOUND('',#1479,.T.);
#1212=FACE_OUTER_BOUND('',#1480,.T.);
#1213=FACE_OUTER_BOUND('',#1481,.T.);
#1214=FACE_OUTER_BOUND('',#1482,.T.);
#1215=FACE_OUTER_BOUND('',#1485,.T.);
#1216=FACE_OUTER_BOUND('',#1488,.T.);
#1217=FACE_OUTER_BOUND('',#1489,.T.);
#1218=FACE_OUTER_BOUND('',#1490,.T.);
#1219=FACE_OUTER_BOUND('',#1491,.T.);
#1220=FACE_OUTER_BOUND('',#1492,.T.);
#1221=FACE_OUTER_BOUND('',#1493,.T.);
#1222=FACE_OUTER_BOUND('',#1494,.T.);
#1223=FACE_OUTER_BOUND('',#1495,.T.);
#1224=FACE_OUTER_BOUND('',#1496,.T.);
#1225=FACE_OUTER_BOUND('',#1497,.T.);
#1226=FACE_OUTER_BOUND('',#1498,.T.);
#1227=FACE_OUTER_BOUND('',#1499,.T.);
#1228=FACE_OUTER_BOUND('',#1500,.T.);
#1229=FACE_OUTER_BOUND('',#1501,.T.);
#1230=FACE_OUTER_BOUND('',#1502,.T.);
#1231=FACE_OUTER_BOUND('',#1503,.T.);
#1232=FACE_OUTER_BOUND('',#1504,.T.);
#1233=FACE_OUTER_BOUND('',#1505,.T.);
#1234=FACE_OUTER_BOUND('',#1506,.T.);
#1235=FACE_OUTER_BOUND('',#1507,.T.);
#1236=FACE_OUTER_BOUND('',#1508,.T.);
#1237=FACE_OUTER_BOUND('',#1510,.T.);
#1238=FACE_OUTER_BOUND('',#1511,.T.);
#1239=FACE_OUTER_BOUND('',#1512,.T.);
#1240=FACE_OUTER_BOUND('',#1513,.T.);
#1241=FACE_OUTER_BOUND('',#1514,.T.);
#1242=FACE_OUTER_BOUND('',#1515,.T.);
#1243=FACE_OUTER_BOUND('',#1517,.T.);
#1244=FACE_OUTER_BOUND('',#1518,.T.);
#1245=FACE_OUTER_BOUND('',#1519,.T.);
#1246=FACE_OUTER_BOUND('',#1521,.T.);
#1247=FACE_OUTER_BOUND('',#1522,.T.);
#1248=FACE_OUTER_BOUND('',#1524,.T.);
#1249=FACE_OUTER_BOUND('',#1525,.T.);
#1250=FACE_OUTER_BOUND('',#1527,.T.);
#1251=FACE_OUTER_BOUND('',#1529,.T.);
#1252=FACE_OUTER_BOUND('',#1531,.T.);
#1253=FACE_OUTER_BOUND('',#1532,.T.);
#1254=FACE_OUTER_BOUND('',#1534,.T.);
#1255=FACE_OUTER_BOUND('',#1536,.T.);
#1256=FACE_OUTER_BOUND('',#1537,.T.);
#1257=FACE_OUTER_BOUND('',#1539,.T.);
#1258=FACE_OUTER_BOUND('',#1540,.T.);
#1259=FACE_OUTER_BOUND('',#1541,.T.);
#1260=FACE_OUTER_BOUND('',#1542,.T.);
#1261=FACE_OUTER_BOUND('',#1543,.T.);
#1262=FACE_OUTER_BOUND('',#1544,.T.);
#1263=FACE_OUTER_BOUND('',#1545,.T.);
#1264=FACE_OUTER_BOUND('',#1546,.T.);
#1265=FACE_OUTER_BOUND('',#1547,.T.);
#1266=FACE_OUTER_BOUND('',#1548,.T.);
#1267=FACE_OUTER_BOUND('',#1549,.T.);
#1268=FACE_OUTER_BOUND('',#1550,.T.);
#1269=FACE_OUTER_BOUND('',#1551,.T.);
#1270=FACE_OUTER_BOUND('',#1552,.T.);
#1271=FACE_OUTER_BOUND('',#1553,.T.);
#1272=FACE_OUTER_BOUND('',#1554,.T.);
#1273=FACE_OUTER_BOUND('',#1555,.T.);
#1274=FACE_OUTER_BOUND('',#1556,.T.);
#1275=FACE_OUTER_BOUND('',#1557,.T.);
#1276=FACE_OUTER_BOUND('',#1558,.T.);
#1277=FACE_OUTER_BOUND('',#1559,.T.);
#1278=FACE_OUTER_BOUND('',#1560,.T.);
#1279=FACE_OUTER_BOUND('',#1561,.T.);
#1280=FACE_OUTER_BOUND('',#1562,.T.);
#1281=FACE_OUTER_BOUND('',#1563,.T.);
#1282=FACE_OUTER_BOUND('',#1564,.T.);
#1283=FACE_OUTER_BOUND('',#1565,.T.);
#1284=FACE_OUTER_BOUND('',#1566,.T.);
#1285=FACE_OUTER_BOUND('',#1567,.T.);
#1286=FACE_OUTER_BOUND('',#1568,.T.);
#1287=FACE_OUTER_BOUND('',#1569,.T.);
#1288=FACE_OUTER_BOUND('',#1570,.T.);
#1289=FACE_OUTER_BOUND('',#1571,.T.);
#1290=FACE_OUTER_BOUND('',#1572,.T.);
#1291=FACE_OUTER_BOUND('',#1573,.T.);
#1292=FACE_OUTER_BOUND('',#1574,.T.);
#1293=FACE_OUTER_BOUND('',#1575,.T.);
#1294=FACE_OUTER_BOUND('',#1576,.T.);
#1295=FACE_OUTER_BOUND('',#1577,.T.);
#1296=FACE_OUTER_BOUND('',#1578,.T.);
#1297=FACE_OUTER_BOUND('',#1579,.T.);
#1298=FACE_OUTER_BOUND('',#1580,.T.);
#1299=FACE_OUTER_BOUND('',#1581,.T.);
#1300=FACE_OUTER_BOUND('',#1582,.T.);
#1301=FACE_OUTER_BOUND('',#1583,.T.);
#1302=FACE_OUTER_BOUND('',#1586,.T.);
#1303=FACE_OUTER_BOUND('',#1589,.T.);
#1304=FACE_OUTER_BOUND('',#1590,.T.);
#1305=FACE_OUTER_BOUND('',#1591,.T.);
#1306=FACE_OUTER_BOUND('',#1592,.T.);
#1307=FACE_OUTER_BOUND('',#1593,.T.);
#1308=FACE_OUTER_BOUND('',#1594,.T.);
#1309=FACE_OUTER_BOUND('',#1595,.T.);
#1310=FACE_OUTER_BOUND('',#1596,.T.);
#1311=FACE_OUTER_BOUND('',#1597,.T.);
#1312=FACE_OUTER_BOUND('',#1598,.T.);
#1313=FACE_OUTER_BOUND('',#1599,.T.);
#1314=FACE_OUTER_BOUND('',#1600,.T.);
#1315=FACE_OUTER_BOUND('',#1603,.T.);
#1316=FACE_OUTER_BOUND('',#1606,.T.);
#1317=FACE_OUTER_BOUND('',#1607,.T.);
#1318=FACE_OUTER_BOUND('',#1608,.T.);
#1319=FACE_OUTER_BOUND('',#1609,.T.);
#1320=FACE_OUTER_BOUND('',#1610,.T.);
#1321=FACE_OUTER_BOUND('',#1611,.T.);
#1322=FACE_OUTER_BOUND('',#1612,.T.);
#1323=FACE_OUTER_BOUND('',#1613,.T.);
#1324=FACE_OUTER_BOUND('',#1614,.T.);
#1325=FACE_OUTER_BOUND('',#1615,.T.);
#1326=FACE_OUTER_BOUND('',#1616,.T.);
#1327=FACE_OUTER_BOUND('',#1617,.T.);
#1328=FACE_OUTER_BOUND('',#1618,.T.);
#1329=EDGE_LOOP('',(#2758,#2759,#2760,#2761));
#1330=EDGE_LOOP('',(#2762,#2763,#2764,#2765));
#1331=EDGE_LOOP('',(#2766,#2767,#2768,#2769));
#1332=EDGE_LOOP('',(#2770,#2771,#2772,#2773));
#1333=EDGE_LOOP('',(#2774,#2775,#2776,#2777));
#1334=EDGE_LOOP('',(#2778,#2779,#2780,#2781));
#1335=EDGE_LOOP('',(#2782,#2783,#2784,#2785));
#1336=EDGE_LOOP('',(#2786,#2787,#2788,#2789));
#1337=EDGE_LOOP('',(#2790,#2791,#2792,#2793));
#1338=EDGE_LOOP('',(#2794,#2795,#2796,#2797));
#1339=EDGE_LOOP('',(#2798,#2799,#2800,#2801));
#1340=EDGE_LOOP('',(#2802,#2803,#2804,#2805));
#1341=EDGE_LOOP('',(#2806,#2807,#2808,#2809));
#1342=EDGE_LOOP('',(#2810,#2811,#2812,#2813));
#1343=EDGE_LOOP('',(#2814,#2815,#2816,#2817,#2818,#2819,#2820,#2821,#2822,
#2823,#2824,#2825,#2826,#2827,#2828,#2829,#2830,#2831,#2832,#2833,#2834,
#2835));
#1344=EDGE_LOOP('',(#2836));
#1345=EDGE_LOOP('',(#2837));
#1346=EDGE_LOOP('',(#2838));
#1347=EDGE_LOOP('',(#2839));
#1348=EDGE_LOOP('',(#2840,#2841,#2842,#2843,#2844,#2845,#2846,#2847,#2848,
#2849,#2850,#2851,#2852));
#1349=EDGE_LOOP('',(#2853,#2854,#2855,#2856,#2857,#2858,#2859,#2860));
#1350=EDGE_LOOP('',(#2861,#2862,#2863,#2864));
#1351=EDGE_LOOP('',(#2865,#2866,#2867,#2868));
#1352=EDGE_LOOP('',(#2869,#2870,#2871,#2872,#2873,#2874,#2875,#2876,#2877,
#2878,#2879,#2880));
#1353=EDGE_LOOP('',(#2881,#2882,#2883,#2884));
#1354=EDGE_LOOP('',(#2885,#2886,#2887,#2888));
#1355=EDGE_LOOP('',(#2889,#2890,#2891,#2892));
#1356=EDGE_LOOP('',(#2893,#2894,#2895,#2896));
#1357=EDGE_LOOP('',(#2897,#2898,#2899,#2900));
#1358=EDGE_LOOP('',(#2901,#2902,#2903,#2904,#2905,#2906,#2907,#2908,#2909,
#2910,#2911,#2912,#2913,#2914,#2915,#2916));
#1359=EDGE_LOOP('',(#2917));
#1360=EDGE_LOOP('',(#2918));
#1361=EDGE_LOOP('',(#2919,#2920,#2921,#2922));
#1362=EDGE_LOOP('',(#2923,#2924,#2925,#2926));
#1363=EDGE_LOOP('',(#2927,#2928,#2929,#2930));
#1364=EDGE_LOOP('',(#2931,#2932,#2933,#2934));
#1365=EDGE_LOOP('',(#2935,#2936,#2937,#2938));
#1366=EDGE_LOOP('',(#2939,#2940,#2941,#2942));
#1367=EDGE_LOOP('',(#2943,#2944,#2945,#2946));
#1368=EDGE_LOOP('',(#2947,#2948,#2949,#2950));
#1369=EDGE_LOOP('',(#2951,#2952,#2953,#2954));
#1370=EDGE_LOOP('',(#2955,#2956,#2957,#2958));
#1371=EDGE_LOOP('',(#2959,#2960,#2961));
#1372=EDGE_LOOP('',(#2962,#2963,#2964));
#1373=EDGE_LOOP('',(#2965,#2966,#2967,#2968));
#1374=EDGE_LOOP('',(#2969,#2970,#2971));
#1375=EDGE_LOOP('',(#2972,#2973,#2974));
#1376=EDGE_LOOP('',(#2975,#2976,#2977,#2978));
#1377=EDGE_LOOP('',(#2979,#2980,#2981,#2982));
#1378=EDGE_LOOP('',(#2983,#2984,#2985,#2986,#2987,#2988));
#1379=EDGE_LOOP('',(#2989,#2990,#2991,#2992,#2993,#2994));
#1380=EDGE_LOOP('',(#2995,#2996,#2997,#2998));
#1381=EDGE_LOOP('',(#2999,#3000,#3001,#3002,#3003));
#1382=EDGE_LOOP('',(#3004,#3005,#3006,#3007,#3008));
#1383=EDGE_LOOP('',(#3009,#3010,#3011,#3012));
#1384=EDGE_LOOP('',(#3013,#3014,#3015,#3016,#3017,#3018,#3019,#3020,#3021,
#3022,#3023,#3024,#3025));
#1385=EDGE_LOOP('',(#3026,#3027,#3028,#3029));
#1386=EDGE_LOOP('',(#3030));
#1387=EDGE_LOOP('',(#3031));
#1388=EDGE_LOOP('',(#3032,#3033,#3034,#3035));
#1389=EDGE_LOOP('',(#3036,#3037,#3038,#3039));
#1390=EDGE_LOOP('',(#3040,#3041,#3042,#3043,#3044,#3045,#3046,#3047,#3048,
#3049));
#1391=EDGE_LOOP('',(#3050,#3051,#3052,#3053));
#1392=EDGE_LOOP('',(#3054));
#1393=EDGE_LOOP('',(#3055,#3056,#3057,#3058,#3059,#3060));
#1394=EDGE_LOOP('',(#3061));
#1395=EDGE_LOOP('',(#3062));
#1396=EDGE_LOOP('',(#3063,#3064,#3065,#3066));
#1397=EDGE_LOOP('',(#3067,#3068,#3069,#3070));
#1398=EDGE_LOOP('',(#3071,#3072,#3073,#3074));
#1399=EDGE_LOOP('',(#3075,#3076,#3077,#3078));
#1400=EDGE_LOOP('',(#3079,#3080,#3081,#3082));
#1401=EDGE_LOOP('',(#3083,#3084,#3085,#3086));
#1402=EDGE_LOOP('',(#3087,#3088,#3089,#3090,#3091,#3092));
#1403=EDGE_LOOP('',(#3093,#3094,#3095,#3096,#3097,#3098));
#1404=EDGE_LOOP('',(#3099));
#1405=EDGE_LOOP('',(#3100,#3101,#3102));
#1406=EDGE_LOOP('',(#3103,#3104,#3105));
#1407=EDGE_LOOP('',(#3106,#3107,#3108));
#1408=EDGE_LOOP('',(#3109,#3110,#3111));
#1409=EDGE_LOOP('',(#3112,#3113,#3114));
#1410=EDGE_LOOP('',(#3115,#3116,#3117,#3118));
#1411=EDGE_LOOP('',(#3119,#3120,#3121,#3122,#3123));
#1412=EDGE_LOOP('',(#3124,#3125,#3126,#3127,#3128));
#1413=EDGE_LOOP('',(#3129,#3130,#3131,#3132,#3133));
#1414=EDGE_LOOP('',(#3134,#3135,#3136,#3137,#3138));
#1415=EDGE_LOOP('',(#3139,#3140,#3141,#3142,#3143));
#1416=EDGE_LOOP('',(#3144,#3145,#3146,#3147,#3148));
#1417=EDGE_LOOP('',(#3149));
#1418=EDGE_LOOP('',(#3150));
#1419=EDGE_LOOP('',(#3151));
#1420=EDGE_LOOP('',(#3152,#3153,#3154,#3155));
#1421=EDGE_LOOP('',(#3156,#3157,#3158,#3159));
#1422=EDGE_LOOP('',(#3160,#3161,#3162,#3163));
#1423=EDGE_LOOP('',(#3164,#3165,#3166,#3167));
#1424=EDGE_LOOP('',(#3168,#3169,#3170,#3171));
#1425=EDGE_LOOP('',(#3172,#3173,#3174,#3175));
#1426=EDGE_LOOP('',(#3176));
#1427=EDGE_LOOP('',(#3177,#3178,#3179,#3180));
#1428=EDGE_LOOP('',(#3181,#3182,#3183,#3184));
#1429=EDGE_LOOP('',(#3185,#3186,#3187,#3188));
#1430=EDGE_LOOP('',(#3189));
#1431=EDGE_LOOP('',(#3190,#3191,#3192,#3193));
#1432=EDGE_LOOP('',(#3194,#3195,#3196,#3197));
#1433=EDGE_LOOP('',(#3198,#3199,#3200,#3201));
#1434=EDGE_LOOP('',(#3202,#3203,#3204,#3205));
#1435=EDGE_LOOP('',(#3206,#3207,#3208,#3209,#3210,#3211,#3212,#3213,#3214,
#3215,#3216,#3217,#3218,#3219,#3220,#3221,#3222,#3223,#3224,#3225));
#1436=EDGE_LOOP('',(#3226));
#1437=EDGE_LOOP('',(#3227,#3228,#3229,#3230,#3231,#3232,#3233,#3234,#3235,
#3236,#3237,#3238,#3239,#3240,#3241,#3242,#3243,#3244,#3245,#3246));
#1438=EDGE_LOOP('',(#3247));
#1439=EDGE_LOOP('',(#3248,#3249,#3250,#3251));
#1440=EDGE_LOOP('',(#3252));
#1441=EDGE_LOOP('',(#3253,#3254,#3255,#3256));
#1442=EDGE_LOOP('',(#3257));
#1443=EDGE_LOOP('',(#3258,#3259,#3260,#3261));
#1444=EDGE_LOOP('',(#3262));
#1445=EDGE_LOOP('',(#3263,#3264,#3265,#3266));
#1446=EDGE_LOOP('',(#3267));
#1447=EDGE_LOOP('',(#3268,#3269,#3270,#3271));
#1448=EDGE_LOOP('',(#3272));
#1449=EDGE_LOOP('',(#3273,#3274,#3275,#3276));
#1450=EDGE_LOOP('',(#3277));
#1451=EDGE_LOOP('',(#3278,#3279,#3280,#3281));
#1452=EDGE_LOOP('',(#3282));
#1453=EDGE_LOOP('',(#3283,#3284,#3285,#3286));
#1454=EDGE_LOOP('',(#3287));
#1455=EDGE_LOOP('',(#3288,#3289,#3290,#3291));
#1456=EDGE_LOOP('',(#3292,#3293,#3294,#3295));
#1457=EDGE_LOOP('',(#3296,#3297));
#1458=EDGE_LOOP('',(#3298,#3299,#3300,#3301));
#1459=EDGE_LOOP('',(#3302,#3303,#3304,#3305));
#1460=EDGE_LOOP('',(#3306,#3307,#3308,#3309));
#1461=EDGE_LOOP('',(#3310,#3311,#3312,#3313));
#1462=EDGE_LOOP('',(#3314,#3315));
#1463=EDGE_LOOP('',(#3316,#3317,#3318,#3319));
#1464=EDGE_LOOP('',(#3320,#3321,#3322,#3323));
#1465=EDGE_LOOP('',(#3324,#3325,#3326,#3327));
#1466=EDGE_LOOP('',(#3328,#3329,#3330,#3331));
#1467=EDGE_LOOP('',(#3332,#3333,#3334,#3335));
#1468=EDGE_LOOP('',(#3336,#3337,#3338,#3339));
#1469=EDGE_LOOP('',(#3340));
#1470=EDGE_LOOP('',(#3341));
#1471=EDGE_LOOP('',(#3342));
#1472=EDGE_LOOP('',(#3343));
#1473=EDGE_LOOP('',(#3344));
#1474=EDGE_LOOP('',(#3345));
#1475=EDGE_LOOP('',(#3346,#3347,#3348,#3349,#3350,#3351));
#1476=EDGE_LOOP('',(#3352,#3353,#3354,#3355,#3356,#3357));
#1477=EDGE_LOOP('',(#3358,#3359,#3360,#3361));
#1478=EDGE_LOOP('',(#3362,#3363,#3364,#3365));
#1479=EDGE_LOOP('',(#3366,#3367,#3368,#3369));
#1480=EDGE_LOOP('',(#3370,#3371,#3372,#3373));
#1481=EDGE_LOOP('',(#3374,#3375,#3376,#3377));
#1482=EDGE_LOOP('',(#3378,#3379,#3380,#3381));
#1483=EDGE_LOOP('',(#3382));
#1484=EDGE_LOOP('',(#3383));
#1485=EDGE_LOOP('',(#3384,#3385,#3386,#3387));
#1486=EDGE_LOOP('',(#3388));
#1487=EDGE_LOOP('',(#3389));
#1488=EDGE_LOOP('',(#3390,#3391,#3392,#3393));
#1489=EDGE_LOOP('',(#3394,#3395,#3396,#3397));
#1490=EDGE_LOOP('',(#3398,#3399,#3400,#3401));
#1491=EDGE_LOOP('',(#3402,#3403,#3404,#3405));
#1492=EDGE_LOOP('',(#3406,#3407,#3408,#3409));
#1493=EDGE_LOOP('',(#3410,#3411,#3412,#3413,#3414));
#1494=EDGE_LOOP('',(#3415,#3416,#3417,#3418,#3419));
#1495=EDGE_LOOP('',(#3420,#3421,#3422,#3423));
#1496=EDGE_LOOP('',(#3424,#3425,#3426,#3427,#3428));
#1497=EDGE_LOOP('',(#3429,#3430,#3431,#3432));
#1498=EDGE_LOOP('',(#3433,#3434,#3435,#3436));
#1499=EDGE_LOOP('',(#3437,#3438,#3439,#3440,#3441));
#1500=EDGE_LOOP('',(#3442,#3443,#3444,#3445));
#1501=EDGE_LOOP('',(#3446,#3447,#3448,#3449,#3450));
#1502=EDGE_LOOP('',(#3451,#3452,#3453,#3454));
#1503=EDGE_LOOP('',(#3455,#3456,#3457,#3458));
#1504=EDGE_LOOP('',(#3459,#3460,#3461,#3462));
#1505=EDGE_LOOP('',(#3463,#3464,#3465,#3466));
#1506=EDGE_LOOP('',(#3467,#3468,#3469,#3470));
#1507=EDGE_LOOP('',(#3471,#3472,#3473,#3474,#3475,#3476,#3477,#3478,#3479,
#3480,#3481,#3482,#3483,#3484,#3485,#3486,#3487,#3488));
#1508=EDGE_LOOP('',(#3489,#3490,#3491,#3492,#3493,#3494,#3495,#3496));
#1509=EDGE_LOOP('',(#3497));
#1510=EDGE_LOOP('',(#3498,#3499,#3500,#3501,#3502,#3503,#3504,#3505));
#1511=EDGE_LOOP('',(#3506,#3507,#3508,#3509,#3510,#3511,#3512,#3513));
#1512=EDGE_LOOP('',(#3514,#3515,#3516,#3517));
#1513=EDGE_LOOP('',(#3518,#3519,#3520,#3521,#3522,#3523,#3524,#3525,#3526,
#3527,#3528,#3529,#3530,#3531,#3532,#3533));
#1514=EDGE_LOOP('',(#3534,#3535,#3536,#3537,#3538,#3539,#3540,#3541,#3542,
#3543,#3544,#3545,#3546,#3547,#3548,#3549));
#1515=EDGE_LOOP('',(#3550,#3551,#3552,#3553));
#1516=EDGE_LOOP('',(#3554));
#1517=EDGE_LOOP('',(#3555,#3556,#3557,#3558));
#1518=EDGE_LOOP('',(#3559,#3560,#3561,#3562));
#1519=EDGE_LOOP('',(#3563,#3564,#3565,#3566));
#1520=EDGE_LOOP('',(#3567));
#1521=EDGE_LOOP('',(#3568,#3569,#3570,#3571));
#1522=EDGE_LOOP('',(#3572,#3573,#3574,#3575));
#1523=EDGE_LOOP('',(#3576));
#1524=EDGE_LOOP('',(#3577,#3578,#3579,#3580));
#1525=EDGE_LOOP('',(#3581));
#1526=EDGE_LOOP('',(#3582));
#1527=EDGE_LOOP('',(#3583,#3584,#3585,#3586,#3587,#3588,#3589,#3590));
#1528=EDGE_LOOP('',(#3591));
#1529=EDGE_LOOP('',(#3592,#3593,#3594,#3595));
#1530=EDGE_LOOP('',(#3596));
#1531=EDGE_LOOP('',(#3597,#3598,#3599,#3600));
#1532=EDGE_LOOP('',(#3601,#3602,#3603,#3604));
#1533=EDGE_LOOP('',(#3605));
#1534=EDGE_LOOP('',(#3606,#3607,#3608,#3609));
#1535=EDGE_LOOP('',(#3610));
#1536=EDGE_LOOP('',(#3611,#3612,#3613,#3614));
#1537=EDGE_LOOP('',(#3615));
#1538=EDGE_LOOP('',(#3616));
#1539=EDGE_LOOP('',(#3617,#3618,#3619,#3620));
#1540=EDGE_LOOP('',(#3621,#3622,#3623,#3624));
#1541=EDGE_LOOP('',(#3625,#3626,#3627,#3628));
#1542=EDGE_LOOP('',(#3629,#3630,#3631,#3632));
#1543=EDGE_LOOP('',(#3633,#3634,#3635,#3636));
#1544=EDGE_LOOP('',(#3637,#3638,#3639,#3640));
#1545=EDGE_LOOP('',(#3641,#3642,#3643,#3644));
#1546=EDGE_LOOP('',(#3645,#3646,#3647,#3648));
#1547=EDGE_LOOP('',(#3649,#3650,#3651,#3652));
#1548=EDGE_LOOP('',(#3653,#3654,#3655,#3656));
#1549=EDGE_LOOP('',(#3657,#3658,#3659,#3660));
#1550=EDGE_LOOP('',(#3661,#3662,#3663,#3664));
#1551=EDGE_LOOP('',(#3665,#3666,#3667,#3668));
#1552=EDGE_LOOP('',(#3669,#3670,#3671));
#1553=EDGE_LOOP('',(#3672,#3673,#3674,#3675));
#1554=EDGE_LOOP('',(#3676,#3677,#3678,#3679));
#1555=EDGE_LOOP('',(#3680,#3681,#3682,#3683));
#1556=EDGE_LOOP('',(#3684,#3685,#3686,#3687));
#1557=EDGE_LOOP('',(#3688,#3689,#3690,#3691));
#1558=EDGE_LOOP('',(#3692,#3693,#3694,#3695));
#1559=EDGE_LOOP('',(#3696,#3697,#3698,#3699));
#1560=EDGE_LOOP('',(#3700,#3701,#3702,#3703));
#1561=EDGE_LOOP('',(#3704,#3705,#3706,#3707));
#1562=EDGE_LOOP('',(#3708,#3709,#3710,#3711));
#1563=EDGE_LOOP('',(#3712,#3713,#3714,#3715));
#1564=EDGE_LOOP('',(#3716,#3717,#3718,#3719));
#1565=EDGE_LOOP('',(#3720,#3721,#3722,#3723));
#1566=EDGE_LOOP('',(#3724,#3725,#3726,#3727));
#1567=EDGE_LOOP('',(#3728,#3729,#3730,#3731));
#1568=EDGE_LOOP('',(#3732,#3733,#3734,#3735));
#1569=EDGE_LOOP('',(#3736,#3737,#3738,#3739));
#1570=EDGE_LOOP('',(#3740,#3741,#3742));
#1571=EDGE_LOOP('',(#3743,#3744,#3745,#3746));
#1572=EDGE_LOOP('',(#3747,#3748,#3749,#3750,#3751));
#1573=EDGE_LOOP('',(#3752,#3753,#3754,#3755));
#1574=EDGE_LOOP('',(#3756,#3757,#3758,#3759));
#1575=EDGE_LOOP('',(#3760,#3761,#3762,#3763));
#1576=EDGE_LOOP('',(#3764));
#1577=EDGE_LOOP('',(#3765));
#1578=EDGE_LOOP('',(#3766));
#1579=EDGE_LOOP('',(#3767));
#1580=EDGE_LOOP('',(#3768,#3769,#3770,#3771));
#1581=EDGE_LOOP('',(#3772,#3773,#3774,#3775));
#1582=EDGE_LOOP('',(#3776,#3777,#3778,#3779));
#1583=EDGE_LOOP('',(#3780,#3781,#3782,#3783));
#1584=EDGE_LOOP('',(#3784));
#1585=EDGE_LOOP('',(#3785));
#1586=EDGE_LOOP('',(#3786,#3787,#3788,#3789));
#1587=EDGE_LOOP('',(#3790));
#1588=EDGE_LOOP('',(#3791));
#1589=EDGE_LOOP('',(#3792,#3793,#3794,#3795));
#1590=EDGE_LOOP('',(#3796,#3797,#3798,#3799));
#1591=EDGE_LOOP('',(#3800,#3801,#3802,#3803));
#1592=EDGE_LOOP('',(#3804,#3805,#3806,#3807,#3808));
#1593=EDGE_LOOP('',(#3809,#3810,#3811,#3812,#3813));
#1594=EDGE_LOOP('',(#3814,#3815,#3816,#3817));
#1595=EDGE_LOOP('',(#3818,#3819,#3820,#3821));
#1596=EDGE_LOOP('',(#3822,#3823,#3824,#3825));
#1597=EDGE_LOOP('',(#3826,#3827,#3828,#3829,#3830));
#1598=EDGE_LOOP('',(#3831,#3832,#3833,#3834));
#1599=EDGE_LOOP('',(#3835,#3836,#3837,#3838,#3839));
#1600=EDGE_LOOP('',(#3840,#3841,#3842,#3843,#3844,#3845,#3846,#3847,#3848));
#1601=EDGE_LOOP('',(#3849));
#1602=EDGE_LOOP('',(#3850));
#1603=EDGE_LOOP('',(#3851,#3852,#3853,#3854,#3855,#3856,#3857,#3858,#3859));
#1604=EDGE_LOOP('',(#3860));
#1605=EDGE_LOOP('',(#3861));
#1606=EDGE_LOOP('',(#3862,#3863,#3864,#3865));
#1607=EDGE_LOOP('',(#3866,#3867,#3868,#3869));
#1608=EDGE_LOOP('',(#3870,#3871,#3872,#3873));
#1609=EDGE_LOOP('',(#3874,#3875,#3876,#3877));
#1610=EDGE_LOOP('',(#3878,#3879,#3880,#3881));
#1611=EDGE_LOOP('',(#3882,#3883,#3884,#3885));
#1612=EDGE_LOOP('',(#3886,#3887,#3888,#3889));
#1613=EDGE_LOOP('',(#3890,#3891,#3892,#3893));
#1614=EDGE_LOOP('',(#3894,#3895,#3896,#3897));
#1615=EDGE_LOOP('',(#3898));
#1616=EDGE_LOOP('',(#3899));
#1617=EDGE_LOOP('',(#3900));
#1618=EDGE_LOOP('',(#3901));
#1619=CIRCLE('',#4253,8.);
#1620=CIRCLE('',#4254,34.);
#1621=CIRCLE('',#4255,8.);
#1622=CIRCLE('',#4256,34.);
#1623=CIRCLE('',#4258,5.00000000000003);
#1624=CIRCLE('',#4259,1.);
#1625=CIRCLE('',#4260,4.00000000000003);
#1626=CIRCLE('',#4262,5.00000000000003);
#1627=CIRCLE('',#4264,5.00000000000003);
#1628=CIRCLE('',#4265,1.);
#1629=CIRCLE('',#4266,4.00000000000003);
#1630=CIRCLE('',#4268,5.00000000000003);
#1631=CIRCLE('',#4270,5.);
#1632=CIRCLE('',#4271,5.);
#1633=CIRCLE('',#4273,5.00000000000002);
#1634=CIRCLE('',#4274,5.00000000000002);
#1635=CIRCLE('',#4276,5.00000000000003);
#1636=CIRCLE('',#4277,5.00000000000003);
#1637=CIRCLE('',#4279,23.5);
#1638=CIRCLE('',#4280,23.5);
#1639=CIRCLE('',#4282,22.);
#1640=CIRCLE('',#4283,22.);
#1641=CIRCLE('',#4285,15.);
#1642=CIRCLE('',#4286,15.);
#1643=CIRCLE('',#4288,55.);
#1644=CIRCLE('',#4289,55.);
#1645=CIRCLE('',#4291,34.);
#1646=CIRCLE('',#4293,34.);
#1647=CIRCLE('',#4295,10.);
#1648=CIRCLE('',#4296,10.);
#1649=CIRCLE('',#4302,31.5);
#1650=CIRCLE('',#4308,10.);
#1651=CIRCLE('',#4309,10.);
#1652=CIRCLE('',#4340,6.);
#1653=CIRCLE('',#4341,6.);
#1654=CIRCLE('',#4343,5.);
#1655=CIRCLE('',#4344,5.);
#1656=CIRCLE('',#4346,10.);
#1657=CIRCLE('',#4347,10.);
#1658=CIRCLE('',#4348,10.);
#1659=CIRCLE('',#4349,10.);
#1660=CIRCLE('',#4350,10.);
#1661=CIRCLE('',#4351,10.);
#1662=CIRCLE('',#4352,10.);
#1663=CIRCLE('',#4353,10.);
#1664=CIRCLE('',#4355,14.);
#1665=CIRCLE('',#4356,14.);
#1666=CIRCLE('',#4383,1.5);
#1667=CIRCLE('',#4384,1.5);
#1668=CIRCLE('',#4386,2.5);
#1669=CIRCLE('',#4387,2.5);
#1670=CIRCLE('',#4389,2.5);
#1671=CIRCLE('',#4390,2.5);
#1672=CIRCLE('',#4392,6.);
#1673=CIRCLE('',#4393,6.);
#1674=CIRCLE('',#4395,10.);
#1675=CIRCLE('',#4396,10.);
#1676=CIRCLE('',#4398,10.);
#1677=CIRCLE('',#4399,10.);
#1678=CIRCLE('',#4401,5.);
#1679=CIRCLE('',#4403,5.);
#1680=CIRCLE('',#4405,5.);
#1681=CIRCLE('',#4406,5.);
#1682=CIRCLE('',#4408,5.);
#1683=CIRCLE('',#4409,5.);
#1684=CIRCLE('',#4412,5.);
#1685=CIRCLE('',#4413,5.);
#1686=CIRCLE('',#4415,5.);
#1687=CIRCLE('',#4416,5.);
#1688=CIRCLE('',#4418,5.);
#1689=CIRCLE('',#4419,5.);
#1690=CIRCLE('',#4421,2.5);
#1691=CIRCLE('',#4422,2.5);
#1692=CIRCLE('',#4426,10.);
#1693=CIRCLE('',#4428,10.);
#1694=CIRCLE('',#4430,10.);
#1695=CIRCLE('',#4432,10.);
#1696=CIRCLE('',#4434,10.);
#1697=CIRCLE('',#4436,10.);
#1698=CIRCLE('',#4438,10.);
#1699=CIRCLE('',#4440,10.);
#1700=CIRCLE('',#4463,5.);
#1701=CIRCLE('',#4464,5.);
#1702=CIRCLE('',#4466,5.);
#1703=CIRCLE('',#4467,5.);
#1704=CIRCLE('',#4469,10.);
#1705=CIRCLE('',#4470,10.);
#1706=CIRCLE('',#4472,10.);
#1707=CIRCLE('',#4474,10.);
#1708=CIRCLE('',#4480,5.);
#1709=CIRCLE('',#4481,3.99999999999998);
#1710=CIRCLE('',#4483,5.);
#1711=CIRCLE('',#4484,3.99999999999998);
#1712=CIRCLE('',#4486,5.);
#1713=CIRCLE('',#4487,5.);
#1714=CIRCLE('',#4488,3.99999999999999);
#1715=CIRCLE('',#4490,5.);
#1716=CIRCLE('',#4491,5.);
#1717=CIRCLE('',#4492,3.99999999999999);
#1718=CIRCLE('',#4494,5.);
#1719=CIRCLE('',#4496,5.);
#1720=CIRCLE('',#4498,5.);
#1721=CIRCLE('',#4499,5.);
#1722=CIRCLE('',#4501,5.);
#1723=CIRCLE('',#4503,5.);
#1724=CIRCLE('',#4505,10.);
#1725=CIRCLE('',#4506,2.);
#1726=CIRCLE('',#4507,8.);
#1727=CIRCLE('',#4508,2.);
#1728=CIRCLE('',#4510,10.);
#1729=CIRCLE('',#4511,2.);
#1730=CIRCLE('',#4512,12.);
#1731=CIRCLE('',#4513,2.);
#1732=CIRCLE('',#4514,10.);
#1733=CIRCLE('',#4516,10.);
#1734=CIRCLE('',#4517,2.);
#1735=CIRCLE('',#4518,8.00000000000001);
#1736=CIRCLE('',#4519,2.);
#1737=CIRCLE('',#4521,5.);
#1738=CIRCLE('',#4522,5.);
#1739=CIRCLE('',#4524,10.);
#1740=CIRCLE('',#4526,5.);
#1741=CIRCLE('',#4527,5.);
#1742=CIRCLE('',#4529,10.);
#1743=CIRCLE('',#4530,10.);
#1744=CIRCLE('',#4532,10.);
#1745=CIRCLE('',#4533,10.);
#1746=CIRCLE('',#4534,10.);
#1747=CIRCLE('',#4535,10.);
#1748=CIRCLE('',#4537,8.);
#1749=CIRCLE('',#4538,22.);
#1750=CIRCLE('',#4542,20.);
#1751=CIRCLE('',#4543,20.);
#1752=CIRCLE('',#4545,5.);
#1753=CIRCLE('',#4546,4.);
#1754=CIRCLE('',#4547,4.);
#1755=CIRCLE('',#4548,5.);
#1756=CIRCLE('',#4550,5.);
#1757=CIRCLE('',#4551,5.);
#1758=CIRCLE('',#4552,4.);
#1759=CIRCLE('',#4553,4.);
#1760=CIRCLE('',#4556,10.);
#1761=CIRCLE('',#4564,12.);
#1762=CIRCLE('',#4565,22.);
#1763=CIRCLE('',#4567,8.00000000000001);
#1764=CIRCLE('',#4569,10.);
#1765=CIRCLE('',#4570,10.);
#1766=CIRCLE('',#4576,7.);
#1767=CIRCLE('',#4577,7.);
#1768=CIRCLE('',#4579,7.);
#1769=CIRCLE('',#4580,7.);
#1770=CIRCLE('',#4582,2.);
#1771=CIRCLE('',#4584,2.);
#1772=CIRCLE('',#4586,2.);
#1773=CIRCLE('',#4588,2.);
#1774=CIRCLE('',#4590,2.);
#1775=CIRCLE('',#4592,2.);
#1776=CIRCLE('',#4593,2.);
#1777=CIRCLE('',#4595,2.);
#1778=CIRCLE('',#4597,2.);
#1779=CIRCLE('',#4599,2.);
#1780=CIRCLE('',#4602,2.);
#1781=CIRCLE('',#4604,2.);
#1782=CIRCLE('',#4606,2.);
#1783=CIRCLE('',#4608,2.);
#1784=CIRCLE('',#4611,2.);
#1785=CIRCLE('',#4612,2.);
#1786=CIRCLE('',#4614,2.);
#1787=CIRCLE('',#4616,2.);
#1788=CIRCLE('',#4618,2.);
#1789=CIRCLE('',#4620,2.);
#1790=CIRCLE('',#4622,2.);
#1791=CIRCLE('',#4624,2.);
#1792=CIRCLE('',#4626,2.);
#1793=CIRCLE('',#4627,2.);
#1794=CIRCLE('',#4629,2.);
#1795=CIRCLE('',#4631,2.);
#1796=CIRCLE('',#4634,2.);
#1797=CIRCLE('',#4635,2.);
#1798=CIRCLE('',#4637,2.);
#1799=CIRCLE('',#4639,2.);
#1800=CIRCLE('',#4648,5.);
#1801=CIRCLE('',#4649,5.);
#1802=CIRCLE('',#4651,5.);
#1803=CIRCLE('',#4652,5.);
#1804=CIRCLE('',#4654,10.);
#1805=CIRCLE('',#4655,10.);
#1806=CIRCLE('',#4657,10.);
#1807=CIRCLE('',#4659,10.);
#1808=CIRCLE('',#4665,5.);
#1809=CIRCLE('',#4666,5.);
#1810=CIRCLE('',#4667,3.99999999999999);
#1811=CIRCLE('',#4669,5.);
#1812=CIRCLE('',#4670,5.);
#1813=CIRCLE('',#4671,3.99999999999999);
#1814=CIRCLE('',#4673,5.);
#1815=CIRCLE('',#4674,3.99999999999998);
#1816=CIRCLE('',#4676,5.);
#1817=CIRCLE('',#4677,3.99999999999998);
#1818=CIRCLE('',#4679,5.);
#1819=CIRCLE('',#4681,5.);
#1820=CIRCLE('',#4683,5.);
#1821=CIRCLE('',#4685,5.);
#1822=VERTEX_POINT('',#6001);
#1823=VERTEX_POINT('',#6002);
#1824=VERTEX_POINT('',#6004);
#1825=VERTEX_POINT('',#6006);
#1826=VERTEX_POINT('',#6010);
#1827=VERTEX_POINT('',#6012);
#1828=VERTEX_POINT('',#6016);
#1829=VERTEX_POINT('',#6020);
#1830=VERTEX_POINT('',#6022);
#1831=VERTEX_POINT('',#6026);
#1832=VERTEX_POINT('',#6030);
#1833=VERTEX_POINT('',#6031);
#1834=VERTEX_POINT('',#6033);
#1835=VERTEX_POINT('',#6035);
#1836=VERTEX_POINT('',#6039);
#1837=VERTEX_POINT('',#6041);
#1838=VERTEX_POINT('',#6045);
#1839=VERTEX_POINT('',#6047);
#1840=VERTEX_POINT('',#6051);
#1841=VERTEX_POINT('',#6052);
#1842=VERTEX_POINT('',#6054);
#1843=VERTEX_POINT('',#6056);
#1844=VERTEX_POINT('',#6060);
#1845=VERTEX_POINT('',#6061);
#1846=VERTEX_POINT('',#6063);
#1847=VERTEX_POINT('',#6065);
#1848=VERTEX_POINT('',#6069);
#1849=VERTEX_POINT('',#6070);
#1850=VERTEX_POINT('',#6072);
#1851=VERTEX_POINT('',#6074);
#1852=VERTEX_POINT('',#6078);
#1853=VERTEX_POINT('',#6079);
#1854=VERTEX_POINT('',#6081);
#1855=VERTEX_POINT('',#6083);
#1856=VERTEX_POINT('',#6087);
#1857=VERTEX_POINT('',#6088);
#1858=VERTEX_POINT('',#6093);
#1859=VERTEX_POINT('',#6095);
#1860=VERTEX_POINT('',#6099);
#1861=VERTEX_POINT('',#6100);
#1862=VERTEX_POINT('',#6102);
#1863=VERTEX_POINT('',#6104);
#1864=VERTEX_POINT('',#6106);
#1865=VERTEX_POINT('',#6108);
#1866=VERTEX_POINT('',#6110);
#1867=VERTEX_POINT('',#6112);
#1868=VERTEX_POINT('',#6114);
#1869=VERTEX_POINT('',#6116);
#1870=VERTEX_POINT('',#6118);
#1871=VERTEX_POINT('',#6120);
#1872=VERTEX_POINT('',#6122);
#1873=VERTEX_POINT('',#6124);
#1874=VERTEX_POINT('',#6126);
#1875=VERTEX_POINT('',#6128);
#1876=VERTEX_POINT('',#6130);
#1877=VERTEX_POINT('',#6132);
#1878=VERTEX_POINT('',#6134);
#1879=VERTEX_POINT('',#6136);
#1880=VERTEX_POINT('',#6138);
#1881=VERTEX_POINT('',#6140);
#1882=VERTEX_POINT('',#6144);
#1883=VERTEX_POINT('',#6152);
#1884=VERTEX_POINT('',#6153);
#1885=VERTEX_POINT('',#6155);
#1886=VERTEX_POINT('',#6157);
#1887=VERTEX_POINT('',#6159);
#1888=VERTEX_POINT('',#6161);
#1889=VERTEX_POINT('',#6166);
#1890=VERTEX_POINT('',#6167);
#1891=VERTEX_POINT('',#6173);
#1892=VERTEX_POINT('',#6175);
#1893=VERTEX_POINT('',#6178);
#1894=VERTEX_POINT('',#6180);
#1895=VERTEX_POINT('',#6183);
#1896=VERTEX_POINT('',#6185);
#1897=VERTEX_POINT('',#6189);
#1898=VERTEX_POINT('',#6202);
#1899=VERTEX_POINT('',#6204);
#1900=VERTEX_POINT('',#6206);
#1901=VERTEX_POINT('',#6209);
#1902=VERTEX_POINT('',#6211);
#1903=VERTEX_POINT('',#6213);
#1904=VERTEX_POINT('',#6215);
#1905=VERTEX_POINT('',#6217);
#1906=VERTEX_POINT('',#6251);
#1907=VERTEX_POINT('',#6254);
#1908=VERTEX_POINT('',#6258);
#1909=VERTEX_POINT('',#6260);
#1910=VERTEX_POINT('',#6262);
#1911=VERTEX_POINT('',#6264);
#1912=VERTEX_POINT('',#6282);
#1913=VERTEX_POINT('',#6284);
#1914=VERTEX_POINT('',#6288);
#1915=VERTEX_POINT('',#6290);
#1916=VERTEX_POINT('',#6294);
#1917=VERTEX_POINT('',#6296);
#1918=VERTEX_POINT('',#6298);
#1919=VERTEX_POINT('',#6300);
#1920=VERTEX_POINT('',#6302);
#1921=VERTEX_POINT('',#6304);
#1922=VERTEX_POINT('',#6306);
#1923=VERTEX_POINT('',#6308);
#1924=VERTEX_POINT('',#6312);
#1925=VERTEX_POINT('',#6314);
#1926=VERTEX_POINT('',#6318);
#1927=VERTEX_POINT('',#6319);
#1928=VERTEX_POINT('',#6321);
#1929=VERTEX_POINT('',#6323);
#1930=VERTEX_POINT('',#6325);
#1931=VERTEX_POINT('',#6327);
#1932=VERTEX_POINT('',#6332);
#1933=VERTEX_POINT('',#6334);
#1934=VERTEX_POINT('',#6338);
#1935=VERTEX_POINT('',#6342);
#1936=VERTEX_POINT('',#6346);
#1937=VERTEX_POINT('',#6350);
#1938=VERTEX_POINT('',#6357);
#1939=VERTEX_POINT('',#6358);
#1940=VERTEX_POINT('',#6360);
#1941=VERTEX_POINT('',#6362);
#1942=VERTEX_POINT('',#6364);
#1943=VERTEX_POINT('',#6366);
#1944=VERTEX_POINT('',#6370);
#1945=VERTEX_POINT('',#6374);
#1946=VERTEX_POINT('',#6378);
#1947=VERTEX_POINT('',#6382);
#1948=VERTEX_POINT('',#6386);
#1949=VERTEX_POINT('',#6390);
#1950=VERTEX_POINT('',#6409);
#1951=VERTEX_POINT('',#6410);
#1952=VERTEX_POINT('',#6412);
#1953=VERTEX_POINT('',#6414);
#1954=VERTEX_POINT('',#6418);
#1955=VERTEX_POINT('',#6419);
#1956=VERTEX_POINT('',#6421);
#1957=VERTEX_POINT('',#6423);
#1958=VERTEX_POINT('',#6427);
#1959=VERTEX_POINT('',#6428);
#1960=VERTEX_POINT('',#6430);
#1961=VERTEX_POINT('',#6432);
#1962=VERTEX_POINT('',#6436);
#1963=VERTEX_POINT('',#6438);
#1964=VERTEX_POINT('',#6442);
#1965=VERTEX_POINT('',#6444);
#1966=VERTEX_POINT('',#6448);
#1967=VERTEX_POINT('',#6450);
#1968=VERTEX_POINT('',#6454);
#1969=VERTEX_POINT('',#6457);
#1970=VERTEX_POINT('',#6461);
#1971=VERTEX_POINT('',#6463);
#1972=VERTEX_POINT('',#6467);
#1973=VERTEX_POINT('',#6469);
#1974=VERTEX_POINT('',#6474);
#1975=VERTEX_POINT('',#6476);
#1976=VERTEX_POINT('',#6480);
#1977=VERTEX_POINT('',#6482);
#1978=VERTEX_POINT('',#6486);
#1979=VERTEX_POINT('',#6488);
#1980=VERTEX_POINT('',#6497);
#1981=VERTEX_POINT('',#6498);
#1982=VERTEX_POINT('',#6500);
#1983=VERTEX_POINT('',#6502);
#1984=VERTEX_POINT('',#6504);
#1985=VERTEX_POINT('',#6506);
#1986=VERTEX_POINT('',#6508);
#1987=VERTEX_POINT('',#6510);
#1988=VERTEX_POINT('',#6512);
#1989=VERTEX_POINT('',#6514);
#1990=VERTEX_POINT('',#6516);
#1991=VERTEX_POINT('',#6518);
#1992=VERTEX_POINT('',#6520);
#1993=VERTEX_POINT('',#6522);
#1994=VERTEX_POINT('',#6524);
#1995=VERTEX_POINT('',#6526);
#1996=VERTEX_POINT('',#6528);
#1997=VERTEX_POINT('',#6530);
#1998=VERTEX_POINT('',#6532);
#1999=VERTEX_POINT('',#6534);
#2000=VERTEX_POINT('',#6538);
#2001=VERTEX_POINT('',#6539);
#2002=VERTEX_POINT('',#6541);
#2003=VERTEX_POINT('',#6543);
#2004=VERTEX_POINT('',#6545);
#2005=VERTEX_POINT('',#6547);
#2006=VERTEX_POINT('',#6549);
#2007=VERTEX_POINT('',#6551);
#2008=VERTEX_POINT('',#6553);
#2009=VERTEX_POINT('',#6555);
#2010=VERTEX_POINT('',#6557);
#2011=VERTEX_POINT('',#6559);
#2012=VERTEX_POINT('',#6561);
#2013=VERTEX_POINT('',#6563);
#2014=VERTEX_POINT('',#6565);
#2015=VERTEX_POINT('',#6567);
#2016=VERTEX_POINT('',#6569);
#2017=VERTEX_POINT('',#6571);
#2018=VERTEX_POINT('',#6573);
#2019=VERTEX_POINT('',#6575);
#2020=VERTEX_POINT('',#6632);
#2021=VERTEX_POINT('',#6634);
#2022=VERTEX_POINT('',#6638);
#2023=VERTEX_POINT('',#6640);
#2024=VERTEX_POINT('',#6644);
#2025=VERTEX_POINT('',#6645);
#2026=VERTEX_POINT('',#6647);
#2027=VERTEX_POINT('',#6649);
#2028=VERTEX_POINT('',#6653);
#2029=VERTEX_POINT('',#6655);
#2030=VERTEX_POINT('',#6659);
#2031=VERTEX_POINT('',#6661);
#2032=VERTEX_POINT('',#6671);
#2033=VERTEX_POINT('',#6673);
#2034=VERTEX_POINT('',#6677);
#2035=VERTEX_POINT('',#6679);
#2036=VERTEX_POINT('',#6683);
#2037=VERTEX_POINT('',#6684);
#2038=VERTEX_POINT('',#6687);
#2039=VERTEX_POINT('',#6691);
#2040=VERTEX_POINT('',#6692);
#2041=VERTEX_POINT('',#6695);
#2042=VERTEX_POINT('',#6699);
#2043=VERTEX_POINT('',#6703);
#2044=VERTEX_POINT('',#6707);
#2045=VERTEX_POINT('',#6709);
#2046=VERTEX_POINT('',#6713);
#2047=VERTEX_POINT('',#6717);
#2048=VERTEX_POINT('',#6721);
#2049=VERTEX_POINT('',#6722);
#2050=VERTEX_POINT('',#6724);
#2051=VERTEX_POINT('',#6726);
#2052=VERTEX_POINT('',#6730);
#2053=VERTEX_POINT('',#6731);
#2054=VERTEX_POINT('',#6733);
#2055=VERTEX_POINT('',#6735);
#2056=VERTEX_POINT('',#6737);
#2057=VERTEX_POINT('',#6741);
#2058=VERTEX_POINT('',#6742);
#2059=VERTEX_POINT('',#6744);
#2060=VERTEX_POINT('',#6746);
#2061=VERTEX_POINT('',#6750);
#2062=VERTEX_POINT('',#6752);
#2063=VERTEX_POINT('',#6756);
#2064=VERTEX_POINT('',#6758);
#2065=VERTEX_POINT('',#6762);
#2066=VERTEX_POINT('',#6764);
#2067=VERTEX_POINT('',#6768);
#2068=VERTEX_POINT('',#6769);
#2069=VERTEX_POINT('',#6771);
#2070=VERTEX_POINT('',#6773);
#2071=VERTEX_POINT('',#6777);
#2072=VERTEX_POINT('',#6779);
#2073=VERTEX_POINT('',#6781);
#2074=VERTEX_POINT('',#6783);
#2075=VERTEX_POINT('',#6833);
#2076=VERTEX_POINT('',#6840);
#2077=VERTEX_POINT('',#6842);
#2078=VERTEX_POINT('',#6898);
#2079=VERTEX_POINT('',#6901);
#2080=VERTEX_POINT('',#6969);
#2081=VERTEX_POINT('',#6971);
#2082=VERTEX_POINT('',#7038);
#2083=VERTEX_POINT('',#7040);
#2084=VERTEX_POINT('',#7042);
#2085=VERTEX_POINT('',#7044);
#2086=VERTEX_POINT('',#7046);
#2087=VERTEX_POINT('',#7048);
#2088=VERTEX_POINT('',#7054);
#2089=VERTEX_POINT('',#7056);
#2090=VERTEX_POINT('',#7060);
#2091=VERTEX_POINT('',#7061);
#2092=VERTEX_POINT('',#7064);
#2093=VERTEX_POINT('',#7066);
#2094=VERTEX_POINT('',#7071);
#2095=VERTEX_POINT('',#7072);
#2096=VERTEX_POINT('',#7077);
#2097=VERTEX_POINT('',#7079);
#2098=VERTEX_POINT('',#7081);
#2099=VERTEX_POINT('',#7083);
#2100=VERTEX_POINT('',#7085);
#2101=VERTEX_POINT('',#7088);
#2102=VERTEX_POINT('',#7090);
#2103=VERTEX_POINT('',#7092);
#2104=VERTEX_POINT('',#7094);
#2105=VERTEX_POINT('',#7096);
#2106=VERTEX_POINT('',#7098);
#2107=VERTEX_POINT('',#7100);
#2108=VERTEX_POINT('',#7102);
#2109=VERTEX_POINT('',#7106);
#2110=VERTEX_POINT('',#7107);
#2111=VERTEX_POINT('',#7110);
#2112=VERTEX_POINT('',#7112);
#2113=VERTEX_POINT('',#7114);
#2114=VERTEX_POINT('',#7116);
#2115=VERTEX_POINT('',#7118);
#2116=VERTEX_POINT('',#7120);
#2117=VERTEX_POINT('',#7122);
#2118=VERTEX_POINT('',#7124);
#2119=VERTEX_POINT('',#7126);
#2120=VERTEX_POINT('',#7129);
#2121=VERTEX_POINT('',#7131);
#2122=VERTEX_POINT('',#7135);
#2123=VERTEX_POINT('',#7136);
#2124=VERTEX_POINT('',#7151);
#2125=VERTEX_POINT('',#7152);
#2126=VERTEX_POINT('',#7154);
#2127=VERTEX_POINT('',#7156);
#2128=VERTEX_POINT('',#7161);
#2129=VERTEX_POINT('',#7163);
#2130=VERTEX_POINT('',#7165);
#2131=VERTEX_POINT('',#7167);
#2132=VERTEX_POINT('',#7169);
#2133=VERTEX_POINT('',#7171);
#2134=VERTEX_POINT('',#7175);
#2135=VERTEX_POINT('',#7176);
#2136=VERTEX_POINT('',#7178);
#2137=VERTEX_POINT('',#7180);
#2138=VERTEX_POINT('',#7189);
#2139=VERTEX_POINT('',#7190);
#2140=VERTEX_POINT('',#7192);
#2141=VERTEX_POINT('',#7194);
#2142=VERTEX_POINT('',#7611);
#2143=VERTEX_POINT('',#7613);
#2144=VERTEX_POINT('',#7617);
#2145=VERTEX_POINT('',#7619);
#2146=VERTEX_POINT('',#7623);
#2147=VERTEX_POINT('',#7624);
#2148=VERTEX_POINT('',#7626);
#2149=VERTEX_POINT('',#7628);
#2150=VERTEX_POINT('',#7632);
#2151=VERTEX_POINT('',#7634);
#2152=VERTEX_POINT('',#7638);
#2153=VERTEX_POINT('',#7640);
#2154=VERTEX_POINT('',#7650);
#2155=VERTEX_POINT('',#7651);
#2156=VERTEX_POINT('',#7654);
#2157=VERTEX_POINT('',#7658);
#2158=VERTEX_POINT('',#7659);
#2159=VERTEX_POINT('',#7662);
#2160=VERTEX_POINT('',#7666);
#2161=VERTEX_POINT('',#7668);
#2162=VERTEX_POINT('',#7672);
#2163=VERTEX_POINT('',#7674);
#2164=VERTEX_POINT('',#7678);
#2165=VERTEX_POINT('',#7682);
#2166=VERTEX_POINT('',#7686);
#2167=VERTEX_POINT('',#7690);
#2168=VERTEX_POINT('',#7694);
#2169=VERTEX_POINT('',#7695);
#2170=VERTEX_POINT('',#7697);
#2171=VERTEX_POINT('',#7699);
#2172=VERTEX_POINT('',#7701);
#2173=VERTEX_POINT('',#7703);
#2174=VERTEX_POINT('',#7705);
#2175=VERTEX_POINT('',#7707);
#2176=VERTEX_POINT('',#7709);
#2177=VERTEX_POINT('',#7713);
#2178=VERTEX_POINT('',#7714);
#2179=VERTEX_POINT('',#7716);
#2180=VERTEX_POINT('',#7718);
#2181=VERTEX_POINT('',#7720);
#2182=VERTEX_POINT('',#7722);
#2183=VERTEX_POINT('',#7724);
#2184=VERTEX_POINT('',#7726);
#2185=VERTEX_POINT('',#7728);
#2186=EDGE_CURVE('',#1822,#1823,#1619,.T.);
#2187=EDGE_CURVE('',#1823,#1824,#1620,.T.);
#2188=EDGE_CURVE('',#1824,#1825,#1621,.T.);
#2189=EDGE_CURVE('',#1822,#1825,#1622,.T.);
#2190=EDGE_CURVE('',#1826,#1826,#1623,.T.);
#2191=EDGE_CURVE('',#1826,#1827,#1624,.T.);
#2192=EDGE_CURVE('',#1827,#1827,#1625,.T.);
#2193=EDGE_CURVE('',#1828,#1828,#1626,.T.);
#2194=EDGE_CURVE('',#1828,#1826,#289,.T.);
#2195=EDGE_CURVE('',#1829,#1829,#1627,.T.);
#2196=EDGE_CURVE('',#1829,#1830,#1628,.T.);
#2197=EDGE_CURVE('',#1830,#1830,#1629,.T.);
#2198=EDGE_CURVE('',#1831,#1831,#1630,.T.);
#2199=EDGE_CURVE('',#1831,#1829,#290,.T.);
#2200=EDGE_CURVE('',#1832,#1833,#1631,.T.);
#2201=EDGE_CURVE('',#1834,#1833,#291,.T.);
#2202=EDGE_CURVE('',#1835,#1834,#1632,.T.);
#2203=EDGE_CURVE('',#1832,#1835,#292,.T.);
#2204=EDGE_CURVE('',#1836,#1836,#1633,.T.);
#2205=EDGE_CURVE('',#1836,#1837,#293,.T.);
#2206=EDGE_CURVE('',#1837,#1837,#1634,.T.);
#2207=EDGE_CURVE('',#1838,#1838,#1635,.T.);
#2208=EDGE_CURVE('',#1838,#1839,#294,.T.);
#2209=EDGE_CURVE('',#1839,#1839,#1636,.T.);
#2210=EDGE_CURVE('',#1840,#1841,#1637,.T.);
#2211=EDGE_CURVE('',#1840,#1842,#295,.T.);
#2212=EDGE_CURVE('',#1842,#1843,#1638,.T.);
#2213=EDGE_CURVE('',#1843,#1841,#296,.T.);
#2214=EDGE_CURVE('',#1844,#1845,#1639,.T.);
#2215=EDGE_CURVE('',#1844,#1846,#297,.T.);
#2216=EDGE_CURVE('',#1846,#1847,#1640,.T.);
#2217=EDGE_CURVE('',#1847,#1845,#298,.T.);
#2218=EDGE_CURVE('',#1848,#1849,#1641,.T.);
#2219=EDGE_CURVE('',#1848,#1850,#299,.T.);
#2220=EDGE_CURVE('',#1850,#1851,#1642,.T.);
#2221=EDGE_CURVE('',#1851,#1849,#300,.T.);
#2222=EDGE_CURVE('',#1852,#1853,#1643,.T.);
#2223=EDGE_CURVE('',#1853,#1854,#301,.T.);
#2224=EDGE_CURVE('',#1855,#1854,#1644,.T.);
#2225=EDGE_CURVE('',#1855,#1852,#302,.T.);
#2226=EDGE_CURVE('',#1856,#1857,#1645,.T.);
#2227=EDGE_CURVE('',#1857,#1824,#303,.T.);
#2228=EDGE_CURVE('',#1823,#1856,#304,.T.);
#2229=EDGE_CURVE('',#1825,#1858,#305,.T.);
#2230=EDGE_CURVE('',#1859,#1858,#1646,.T.);
#2231=EDGE_CURVE('',#1859,#1822,#306,.T.);
#2232=EDGE_CURVE('',#1860,#1861,#307,.T.);
#2233=EDGE_CURVE('',#1862,#1860,#308,.T.);
#2234=EDGE_CURVE('',#1862,#1863,#309,.T.);
#2235=EDGE_CURVE('',#1863,#1864,#310,.T.);
#2236=EDGE_CURVE('',#1864,#1865,#311,.T.);
#2237=EDGE_CURVE('',#1865,#1866,#1647,.T.);
#2238=EDGE_CURVE('',#1866,#1867,#312,.T.);
#2239=EDGE_CURVE('',#1867,#1868,#313,.T.);
#2240=EDGE_CURVE('',#1868,#1869,#314,.T.);
#2241=EDGE_CURVE('',#1870,#1869,#315,.T.);
#2242=EDGE_CURVE('',#1870,#1871,#316,.T.);
#2243=EDGE_CURVE('',#1871,#1872,#317,.T.);
#2244=EDGE_CURVE('',#1872,#1873,#318,.T.);
#2245=EDGE_CURVE('',#1874,#1873,#319,.T.);
#2246=EDGE_CURVE('',#1875,#1874,#320,.T.);
#2247=EDGE_CURVE('',#1875,#1876,#321,.T.);
#2248=EDGE_CURVE('',#1876,#1877,#322,.T.);
#2249=EDGE_CURVE('',#1877,#1878,#323,.T.);
#2250=EDGE_CURVE('',#1878,#1879,#324,.T.);
#2251=EDGE_CURVE('',#1879,#1880,#1648,.T.);
#2252=EDGE_CURVE('',#1880,#1881,#325,.T.);
#2253=EDGE_CURVE('',#1881,#1861,#326,.T.);
#2254=EDGE_CURVE('',#1858,#1882,#327,.T.);
#2255=EDGE_CURVE('',#1854,#1857,#328,.T.);
#2256=EDGE_CURVE('',#1849,#1853,#329,.T.);
#2257=EDGE_CURVE('',#1845,#1851,#330,.T.);
#2258=EDGE_CURVE('',#1841,#1847,#331,.T.);
#2259=EDGE_CURVE('',#1882,#1843,#332,.T.);
#2260=EDGE_CURVE('',#1883,#1884,#333,.T.);
#2261=EDGE_CURVE('',#1885,#1884,#334,.T.);
#2262=EDGE_CURVE('',#1886,#1885,#335,.T.);
#2263=EDGE_CURVE('',#1886,#1887,#336,.T.);
#2264=EDGE_CURVE('',#1887,#1888,#337,.T.);
#2265=EDGE_CURVE('',#1888,#1862,#338,.T.);
#2266=EDGE_CURVE('',#1860,#1883,#339,.T.);
#2267=EDGE_CURVE('',#1889,#1890,#340,.T.);
#2268=EDGE_CURVE('',#1861,#1890,#341,.T.);
#2269=EDGE_CURVE('',#1881,#1889,#342,.T.);
#2270=EDGE_CURVE('',#1852,#1848,#343,.T.);
#2271=EDGE_CURVE('',#1876,#1891,#344,.T.);
#2272=EDGE_CURVE('',#1891,#1892,#345,.T.);
#2273=EDGE_CURVE('',#1873,#1892,#346,.T.);
#2274=EDGE_CURVE('',#1872,#1893,#347,.T.);
#2275=EDGE_CURVE('',#1894,#1893,#348,.T.);
#2276=EDGE_CURVE('',#1869,#1894,#349,.T.);
#2277=EDGE_CURVE('',#1868,#1895,#350,.T.);
#2278=EDGE_CURVE('',#1895,#1896,#351,.T.);
#2279=EDGE_CURVE('',#1877,#1896,#352,.T.);
#2280=EDGE_CURVE('',#1897,#1882,#1649,.T.);
#2281=EDGE_CURVE('',#1842,#1897,#353,.T.);
#2282=EDGE_CURVE('',#1897,#1859,#354,.T.);
#2283=EDGE_CURVE('',#1856,#1855,#355,.T.);
#2284=EDGE_CURVE('',#1850,#1844,#356,.T.);
#2285=EDGE_CURVE('',#1846,#1840,#357,.T.);
#2286=EDGE_CURVE('',#1883,#1890,#358,.T.);
#2287=EDGE_CURVE('',#1898,#1889,#359,.T.);
#2288=EDGE_CURVE('',#1899,#1898,#1650,.T.);
#2289=EDGE_CURVE('',#1900,#1899,#360,.T.);
#2290=EDGE_CURVE('',#1896,#1900,#361,.T.);
#2291=EDGE_CURVE('',#1901,#1895,#362,.T.);
#2292=EDGE_CURVE('',#1902,#1901,#363,.T.);
#2293=EDGE_CURVE('',#1903,#1902,#1651,.T.);
#2294=EDGE_CURVE('',#1904,#1903,#364,.T.);
#2295=EDGE_CURVE('',#1905,#1904,#365,.T.);
#2296=EDGE_CURVE('',#1905,#1888,#366,.T.);
#2297=EDGE_CURVE('',#1884,#1887,#367,.T.);
#2298=EDGE_CURVE('',#1878,#1900,#368,.T.);
#2299=EDGE_CURVE('',#1879,#1899,#369,.T.);
#2300=EDGE_CURVE('',#1880,#1898,#370,.T.);
#2301=EDGE_CURVE('',#1905,#1863,#371,.T.);
#2302=EDGE_CURVE('',#1864,#1904,#372,.T.);
#2303=EDGE_CURVE('',#1865,#1903,#373,.T.);
#2304=EDGE_CURVE('',#1866,#1902,#374,.T.);
#2305=EDGE_CURVE('',#1867,#1901,#375,.T.);
#2306=EDGE_CURVE('',#1893,#1871,#376,.T.);
#2307=EDGE_CURVE('',#1894,#1870,#377,.T.);
#2308=EDGE_CURVE('',#1892,#1874,#378,.T.);
#2309=EDGE_CURVE('',#1891,#1875,#379,.T.);
#2310=EDGE_CURVE('',#1906,#1887,#380,.T.);
#2311=EDGE_CURVE('',#1906,#1835,#381,.T.);
#2312=EDGE_CURVE('',#1834,#1907,#382,.T.);
#2313=EDGE_CURVE('',#1884,#1907,#383,.T.);
#2314=EDGE_CURVE('',#1908,#1832,#384,.T.);
#2315=EDGE_CURVE('',#1908,#1909,#385,.T.);
#2316=EDGE_CURVE('',#1909,#1910,#386,.T.);
#2317=EDGE_CURVE('',#1910,#1911,#387,.T.);
#2318=EDGE_CURVE('',#1833,#1911,#388,.T.);
#2319=EDGE_CURVE('',#1910,#1885,#389,.T.);
#2320=EDGE_CURVE('',#1909,#1886,#390,.T.);
#2321=EDGE_CURVE('',#1907,#1911,#391,.T.);
#2322=EDGE_CURVE('',#1908,#1906,#392,.T.);
#2323=EDGE_CURVE('',#1912,#1912,#1652,.T.);
#2324=EDGE_CURVE('',#1912,#1913,#393,.T.);
#2325=EDGE_CURVE('',#1913,#1913,#1653,.T.);
#2326=EDGE_CURVE('',#1914,#1914,#1654,.T.);
#2327=EDGE_CURVE('',#1914,#1915,#394,.T.);
#2328=EDGE_CURVE('',#1915,#1915,#1655,.T.);
#2329=EDGE_CURVE('',#1916,#1916,#1656,.T.);
#2330=EDGE_CURVE('',#1916,#1917,#395,.T.);
#2331=EDGE_CURVE('',#1918,#1917,#1657,.T.);
#2332=EDGE_CURVE('',#1919,#1918,#1658,.T.);
#2333=EDGE_CURVE('',#1920,#1919,#1659,.T.);
#2334=EDGE_CURVE('',#1921,#1920,#1660,.T.);
#2335=EDGE_CURVE('',#1921,#1922,#1661,.T.);
#2336=EDGE_CURVE('',#1923,#1922,#1662,.T.);
#2337=EDGE_CURVE('',#1917,#1923,#1663,.T.);
#2338=EDGE_CURVE('',#1924,#1924,#1664,.T.);
#2339=EDGE_CURVE('',#1924,#1925,#396,.T.);
#2340=EDGE_CURVE('',#1925,#1925,#1665,.T.);
#2341=EDGE_CURVE('',#1926,#1927,#397,.T.);
#2342=EDGE_CURVE('',#1928,#1926,#398,.T.);
#2343=EDGE_CURVE('',#1929,#1928,#399,.T.);
#2344=EDGE_CURVE('',#1930,#1929,#400,.T.);
#2345=EDGE_CURVE('',#1931,#1930,#401,.T.);
#2346=EDGE_CURVE('',#1927,#1931,#402,.T.);
#2347=EDGE_CURVE('',#1932,#1926,#403,.T.);
#2348=EDGE_CURVE('',#1933,#1932,#404,.T.);
#2349=EDGE_CURVE('',#1933,#1928,#405,.T.);
#2350=EDGE_CURVE('',#1934,#1933,#406,.T.);
#2351=EDGE_CURVE('',#1934,#1929,#407,.T.);
#2352=EDGE_CURVE('',#1935,#1934,#408,.T.);
#2353=EDGE_CURVE('',#1935,#1930,#409,.T.);
#2354=EDGE_CURVE('',#1936,#1935,#410,.T.);
#2355=EDGE_CURVE('',#1936,#1931,#411,.T.);
#2356=EDGE_CURVE('',#1937,#1936,#412,.T.);
#2357=EDGE_CURVE('',#1937,#1927,#413,.T.);
#2358=EDGE_CURVE('',#1932,#1937,#414,.T.);
#2359=EDGE_CURVE('',#1938,#1939,#415,.T.);
#2360=EDGE_CURVE('',#1939,#1940,#416,.T.);
#2361=EDGE_CURVE('',#1940,#1941,#417,.T.);
#2362=EDGE_CURVE('',#1941,#1942,#418,.T.);
#2363=EDGE_CURVE('',#1942,#1943,#419,.T.);
#2364=EDGE_CURVE('',#1943,#1938,#420,.T.);
#2365=EDGE_CURVE('',#1923,#1944,#421,.T.);
#2366=EDGE_CURVE('',#1944,#1922,#422,.T.);
#2367=EDGE_CURVE('',#1922,#1945,#423,.T.);
#2368=EDGE_CURVE('',#1945,#1921,#424,.T.);
#2369=EDGE_CURVE('',#1921,#1946,#425,.T.);
#2370=EDGE_CURVE('',#1946,#1920,#426,.T.);
#2371=EDGE_CURVE('',#1920,#1947,#427,.T.);
#2372=EDGE_CURVE('',#1947,#1919,#428,.T.);
#2373=EDGE_CURVE('',#1919,#1948,#429,.T.);
#2374=EDGE_CURVE('',#1948,#1918,#430,.T.);
#2375=EDGE_CURVE('',#1918,#1949,#431,.T.);
#2376=EDGE_CURVE('',#1949,#1923,#432,.T.);
#2377=EDGE_CURVE('',#1939,#1948,#433,.T.);
#2378=EDGE_CURVE('',#1938,#1947,#434,.T.);
#2379=EDGE_CURVE('',#1940,#1949,#435,.T.);
#2380=EDGE_CURVE('',#1941,#1944,#436,.T.);
#2381=EDGE_CURVE('',#1942,#1945,#437,.T.);
#2382=EDGE_CURVE('',#1943,#1946,#438,.T.);
#2383=EDGE_CURVE('',#1950,#1951,#1666,.T.);
#2384=EDGE_CURVE('',#1950,#1952,#439,.T.);
#2385=EDGE_CURVE('',#1952,#1953,#1667,.T.);
#2386=EDGE_CURVE('',#1951,#1953,#440,.T.);
#2387=EDGE_CURVE('',#1954,#1955,#1668,.T.);
#2388=EDGE_CURVE('',#1954,#1956,#441,.T.);
#2389=EDGE_CURVE('',#1956,#1957,#1669,.T.);
#2390=EDGE_CURVE('',#1955,#1957,#442,.T.);
#2391=EDGE_CURVE('',#1958,#1959,#1670,.T.);
#2392=EDGE_CURVE('',#1958,#1960,#443,.T.);
#2393=EDGE_CURVE('',#1960,#1961,#1671,.T.);
#2394=EDGE_CURVE('',#1959,#1961,#444,.T.);
#2395=EDGE_CURVE('',#1962,#1962,#1672,.T.);
#2396=EDGE_CURVE('',#1962,#1963,#445,.T.);
#2397=EDGE_CURVE('',#1963,#1963,#1673,.T.);
#2398=EDGE_CURVE('',#1964,#1964,#1674,.T.);
#2399=EDGE_CURVE('',#1964,#1965,#446,.T.);
#2400=EDGE_CURVE('',#1965,#1965,#1675,.T.);
#2401=EDGE_CURVE('',#1966,#1966,#1676,.T.);
#2402=EDGE_CURVE('',#1966,#1967,#447,.T.);
#2403=EDGE_CURVE('',#1967,#1967,#1677,.T.);
#2404=EDGE_CURVE('',#1968,#1968,#1678,.T.);
#2405=EDGE_CURVE('',#1969,#1969,#1679,.T.);
#2406=EDGE_CURVE('',#1969,#1968,#448,.T.);
#2407=EDGE_CURVE('',#1970,#1970,#1680,.T.);
#2408=EDGE_CURVE('',#1970,#1971,#449,.T.);
#2409=EDGE_CURVE('',#1971,#1971,#1681,.T.);
#2410=EDGE_CURVE('',#1972,#1972,#1682,.T.);
#2411=EDGE_CURVE('',#1972,#1973,#450,.T.);
#2412=EDGE_CURVE('',#1973,#1973,#1683,.T.);
#2413=EDGE_CURVE('',#1974,#1974,#1684,.T.);
#2414=EDGE_CURVE('',#1974,#1975,#451,.T.);
#2415=EDGE_CURVE('',#1975,#1975,#1685,.T.);
#2416=EDGE_CURVE('',#1976,#1976,#1686,.T.);
#2417=EDGE_CURVE('',#1976,#1977,#452,.T.);
#2418=EDGE_CURVE('',#1977,#1977,#1687,.T.);
#2419=EDGE_CURVE('',#1978,#1978,#1688,.T.);
#2420=EDGE_CURVE('',#1978,#1979,#453,.T.);
#2421=EDGE_CURVE('',#1979,#1979,#1689,.T.);
#2422=EDGE_CURVE('',#1959,#1958,#1690,.T.);
#2423=EDGE_CURVE('',#1957,#1959,#454,.T.);
#2424=EDGE_CURVE('',#1957,#1956,#1691,.T.);
#2425=EDGE_CURVE('',#1958,#1956,#455,.T.);
#2426=EDGE_CURVE('',#1980,#1981,#456,.T.);
#2427=EDGE_CURVE('',#1981,#1982,#457,.T.);
#2428=EDGE_CURVE('',#1982,#1983,#458,.T.);
#2429=EDGE_CURVE('',#1983,#1984,#459,.T.);
#2430=EDGE_CURVE('',#1984,#1985,#460,.T.);
#2431=EDGE_CURVE('',#1985,#1986,#461,.T.);
#2432=EDGE_CURVE('',#1986,#1987,#462,.T.);
#2433=EDGE_CURVE('',#1987,#1988,#463,.T.);
#2434=EDGE_CURVE('',#1988,#1989,#464,.T.);
#2435=EDGE_CURVE('',#1989,#1990,#465,.T.);
#2436=EDGE_CURVE('',#1990,#1991,#466,.T.);
#2437=EDGE_CURVE('',#1992,#1991,#467,.T.);
#2438=EDGE_CURVE('',#1992,#1993,#468,.T.);
#2439=EDGE_CURVE('',#1993,#1994,#469,.T.);
#2440=EDGE_CURVE('',#1994,#1995,#470,.T.);
#2441=EDGE_CURVE('',#1996,#1995,#471,.T.);
#2442=EDGE_CURVE('',#1996,#1997,#472,.T.);
#2443=EDGE_CURVE('',#1997,#1998,#473,.T.);
#2444=EDGE_CURVE('',#1998,#1999,#474,.T.);
#2445=EDGE_CURVE('',#1999,#1980,#475,.T.);
#2446=EDGE_CURVE('',#2000,#2001,#476,.T.);
#2447=EDGE_CURVE('',#2002,#2000,#477,.T.);
#2448=EDGE_CURVE('',#2003,#2002,#478,.T.);
#2449=EDGE_CURVE('',#2004,#2003,#479,.T.);
#2450=EDGE_CURVE('',#2005,#2004,#480,.T.);
#2451=EDGE_CURVE('',#2006,#2005,#481,.T.);
#2452=EDGE_CURVE('',#2006,#2007,#482,.T.);
#2453=EDGE_CURVE('',#2008,#2007,#483,.T.);
#2454=EDGE_CURVE('',#2009,#2008,#484,.T.);
#2455=EDGE_CURVE('',#2010,#2009,#485,.T.);
#2456=EDGE_CURVE('',#2010,#2011,#486,.T.);
#2457=EDGE_CURVE('',#2012,#2011,#487,.T.);
#2458=EDGE_CURVE('',#2013,#2012,#488,.T.);
#2459=EDGE_CURVE('',#2014,#2013,#489,.T.);
#2460=EDGE_CURVE('',#2015,#2014,#490,.T.);
#2461=EDGE_CURVE('',#2016,#2015,#491,.T.);
#2462=EDGE_CURVE('',#2017,#2016,#492,.T.);
#2463=EDGE_CURVE('',#2018,#2017,#493,.T.);
#2464=EDGE_CURVE('',#2019,#2018,#494,.T.);
#2465=EDGE_CURVE('',#2001,#2019,#495,.T.);
#2466=EDGE_CURVE('',#1991,#2011,#1692,.T.);
#2467=EDGE_CURVE('',#1990,#2012,#496,.T.);
#2468=EDGE_CURVE('',#2010,#1992,#1693,.T.);
#2469=EDGE_CURVE('',#1993,#2009,#497,.T.);
#2470=EDGE_CURVE('',#1995,#2007,#1694,.T.);
#2471=EDGE_CURVE('',#1994,#2008,#498,.T.);
#2472=EDGE_CURVE('',#2006,#1996,#1695,.T.);
#2473=EDGE_CURVE('',#1997,#2005,#499,.T.);
#2474=EDGE_CURVE('',#1981,#2000,#1696,.T.);
#2475=EDGE_CURVE('',#1980,#2002,#500,.T.);
#2476=EDGE_CURVE('',#2001,#1982,#1697,.T.);
#2477=EDGE_CURVE('',#1983,#2019,#501,.T.);
#2478=EDGE_CURVE('',#1985,#2017,#1698,.T.);
#2479=EDGE_CURVE('',#1984,#2018,#502,.T.);
#2480=EDGE_CURVE('',#2016,#1986,#1699,.T.);
#2481=EDGE_CURVE('',#1987,#2015,#503,.T.);
#2482=EDGE_CURVE('',#1988,#2014,#504,.T.);
#2483=EDGE_CURVE('',#1989,#2013,#505,.T.);
#2484=EDGE_CURVE('',#1998,#2004,#506,.T.);
#2485=EDGE_CURVE('',#1999,#2003,#507,.T.);
#2486=EDGE_CURVE('',#1953,#1960,#508,.T.);
#2487=EDGE_CURVE('',#1951,#1954,#509,.T.);
#2488=EDGE_CURVE('',#1961,#1952,#510,.T.);
#2489=EDGE_CURVE('',#1955,#1950,#511,.T.);
#2490=EDGE_CURVE('',#2020,#2020,#1700,.T.);
#2491=EDGE_CURVE('',#2020,#2021,#512,.T.);
#2492=EDGE_CURVE('',#2021,#2021,#1701,.T.);
#2493=EDGE_CURVE('',#2022,#2022,#1702,.T.);
#2494=EDGE_CURVE('',#2022,#2023,#513,.T.);
#2495=EDGE_CURVE('',#2023,#2023,#1703,.T.);
#2496=EDGE_CURVE('',#2024,#2025,#1704,.T.);
#2497=EDGE_CURVE('',#2024,#2026,#514,.T.);
#2498=EDGE_CURVE('',#2026,#2027,#1705,.T.);
#2499=EDGE_CURVE('',#2025,#2027,#515,.T.);
#2500=EDGE_CURVE('',#2025,#2028,#516,.T.);
#2501=EDGE_CURVE('',#2028,#2029,#1706,.T.);
#2502=EDGE_CURVE('',#2029,#2024,#517,.T.);
#2503=EDGE_CURVE('',#2030,#2026,#518,.T.);
#2504=EDGE_CURVE('',#2031,#2030,#1707,.T.);
#2505=EDGE_CURVE('',#2027,#2031,#519,.T.);
#2506=EDGE_CURVE('',#2028,#2031,#520,.T.);
#2507=EDGE_CURVE('',#2029,#2030,#521,.T.);
#2508=EDGE_CURVE('',#2032,#2032,#1708,.T.);
#2509=EDGE_CURVE('',#2032,#2033,#522,.T.);
#2510=EDGE_CURVE('',#2033,#2033,#1709,.T.);
#2511=EDGE_CURVE('',#2034,#2034,#1710,.T.);
#2512=EDGE_CURVE('',#2034,#2035,#523,.T.);
#2513=EDGE_CURVE('',#2035,#2035,#1711,.T.);
#2514=EDGE_CURVE('',#2036,#2037,#1712,.T.);
#2515=EDGE_CURVE('',#2037,#2036,#1713,.T.);
#2516=EDGE_CURVE('',#2037,#2038,#524,.T.);
#2517=EDGE_CURVE('',#2038,#2038,#1714,.T.);
#2518=EDGE_CURVE('',#2039,#2040,#1715,.T.);
#2519=EDGE_CURVE('',#2040,#2039,#1716,.T.);
#2520=EDGE_CURVE('',#2040,#2041,#525,.T.);
#2521=EDGE_CURVE('',#2041,#2041,#1717,.T.);
#2522=EDGE_CURVE('',#2042,#2042,#1718,.T.);
#2523=EDGE_CURVE('',#2042,#2034,#526,.T.);
#2524=EDGE_CURVE('',#2039,#2043,#527,.T.);
#2525=EDGE_CURVE('',#2043,#2043,#1719,.T.);
#2526=EDGE_CURVE('',#2044,#2044,#1720,.T.);
#2527=EDGE_CURVE('',#2044,#2045,#528,.T.);
#2528=EDGE_CURVE('',#2045,#2045,#1721,.T.);
#2529=EDGE_CURVE('',#2046,#2046,#1722,.T.);
#2530=EDGE_CURVE('',#2046,#2032,#529,.T.);
#2531=EDGE_CURVE('',#2036,#2047,#530,.T.);
#2532=EDGE_CURVE('',#2047,#2047,#1723,.T.);
#2533=EDGE_CURVE('',#2048,#2049,#1724,.T.);
#2534=EDGE_CURVE('',#2050,#2048,#1725,.T.);
#2535=EDGE_CURVE('',#2051,#2050,#1726,.T.);
#2536=EDGE_CURVE('',#2051,#2049,#1727,.T.);
#2537=EDGE_CURVE('',#2052,#2053,#1728,.T.);
#2538=EDGE_CURVE('',#2054,#2052,#1729,.T.);
#2539=EDGE_CURVE('',#2055,#2054,#1730,.T.);
#2540=EDGE_CURVE('',#2055,#2056,#1731,.T.);
#2541=EDGE_CURVE('',#2053,#2056,#1732,.T.);
#2542=EDGE_CURVE('',#2057,#2058,#1733,.T.);
#2543=EDGE_CURVE('',#2059,#2057,#1734,.T.);
#2544=EDGE_CURVE('',#2060,#2059,#1735,.T.);
#2545=EDGE_CURVE('',#2058,#2060,#1736,.T.);
#2546=EDGE_CURVE('',#2061,#2061,#1737,.T.);
#2547=EDGE_CURVE('',#2061,#2062,#531,.T.);
#2548=EDGE_CURVE('',#2062,#2062,#1738,.T.);
#2549=EDGE_CURVE('',#2049,#2063,#532,.T.);
#2550=EDGE_CURVE('',#2064,#2063,#1739,.T.);
#2551=EDGE_CURVE('',#2048,#2064,#533,.T.);
#2552=EDGE_CURVE('',#2065,#2065,#1740,.T.);
#2553=EDGE_CURVE('',#2065,#2066,#534,.T.);
#2554=EDGE_CURVE('',#2066,#2066,#1741,.T.);
#2555=EDGE_CURVE('',#2067,#2068,#1742,.T.);
#2556=EDGE_CURVE('',#2068,#2069,#535,.T.);
#2557=EDGE_CURVE('',#2069,#2070,#1743,.T.);
#2558=EDGE_CURVE('',#2067,#2070,#536,.T.);
#2559=EDGE_CURVE('',#2071,#2071,#1744,.T.);
#2560=EDGE_CURVE('',#2071,#2072,#537,.T.);
#2561=EDGE_CURVE('',#2072,#2073,#1745,.T.);
#2562=EDGE_CURVE('',#2073,#2074,#15,.T.);
#2563=EDGE_CURVE('',#2074,#2075,#16,.T.);
#2564=EDGE_CURVE('',#2076,#2075,#538,.T.);
#2565=EDGE_CURVE('',#2076,#2077,#17,.T.);
#2566=EDGE_CURVE('',#2077,#2052,#18,.T.);
#2567=EDGE_CURVE('',#2053,#2078,#539,.T.);
#2568=EDGE_CURVE('',#2078,#2078,#1746,.T.);
#2569=EDGE_CURVE('',#2056,#2079,#19,.T.);
#2570=EDGE_CURVE('',#2079,#2080,#540,.T.);
#2571=EDGE_CURVE('',#2080,#2081,#20,.T.);
#2572=EDGE_CURVE('',#2081,#2072,#1747,.T.);
#2573=EDGE_CURVE('',#2054,#2082,#541,.T.);
#2574=EDGE_CURVE('',#2082,#2083,#1748,.T.);
#2575=EDGE_CURVE('',#2083,#2084,#542,.T.);
#2576=EDGE_CURVE('',#2084,#2085,#1749,.T.);
#2577=EDGE_CURVE('',#2085,#2086,#543,.T.);
#2578=EDGE_CURVE('',#2086,#2087,#544,.T.);
#2579=EDGE_CURVE('',#2087,#2055,#545,.T.);
#2580=EDGE_CURVE('',#2068,#2076,#546,.T.);
#2581=EDGE_CURVE('',#2075,#2048,#547,.T.);
#2582=EDGE_CURVE('',#2088,#2064,#548,.T.);
#2583=EDGE_CURVE('',#2089,#2088,#549,.T.);
#2584=EDGE_CURVE('',#2089,#2069,#550,.T.);
#2585=EDGE_CURVE('',#2090,#2091,#551,.T.);
#2586=EDGE_CURVE('',#2090,#2067,#552,.T.);
#2587=EDGE_CURVE('',#2070,#2092,#553,.T.);
#2588=EDGE_CURVE('',#2092,#2093,#554,.T.);
#2589=EDGE_CURVE('',#2063,#2093,#555,.T.);
#2590=EDGE_CURVE('',#2049,#2091,#556,.T.);
#2591=EDGE_CURVE('',#2094,#2095,#557,.T.);
#2592=EDGE_CURVE('',#2094,#2090,#1750,.T.);
#2593=EDGE_CURVE('',#2091,#2095,#1751,.T.);
#2594=EDGE_CURVE('',#2058,#2096,#558,.T.);
#2595=EDGE_CURVE('',#2058,#2097,#559,.T.);
#2596=EDGE_CURVE('',#2097,#2098,#1752,.T.);
#2597=EDGE_CURVE('',#2098,#2099,#560,.T.);
#2598=EDGE_CURVE('',#2100,#2099,#1753,.T.);
#2599=EDGE_CURVE('',#2100,#2094,#561,.T.);
#2600=EDGE_CURVE('',#2095,#2101,#562,.T.);
#2601=EDGE_CURVE('',#2102,#2101,#1754,.T.);
#2602=EDGE_CURVE('',#2102,#2103,#563,.T.);
#2603=EDGE_CURVE('',#2103,#2104,#1755,.T.);
#2604=EDGE_CURVE('',#2104,#2105,#564,.T.);
#2605=EDGE_CURVE('',#2105,#2106,#565,.T.);
#2606=EDGE_CURVE('',#2107,#2106,#566,.T.);
#2607=EDGE_CURVE('',#2108,#2107,#567,.T.);
#2608=EDGE_CURVE('',#2108,#2096,#568,.T.);
#2609=EDGE_CURVE('',#2109,#2110,#1756,.T.);
#2610=EDGE_CURVE('',#2110,#2057,#569,.T.);
#2611=EDGE_CURVE('',#2057,#2111,#570,.T.);
#2612=EDGE_CURVE('',#2111,#2112,#571,.T.);
#2613=EDGE_CURVE('',#2112,#2113,#572,.T.);
#2614=EDGE_CURVE('',#2114,#2113,#573,.T.);
#2615=EDGE_CURVE('',#2115,#2114,#574,.T.);
#2616=EDGE_CURVE('',#2115,#2116,#575,.T.);
#2617=EDGE_CURVE('',#2116,#2117,#1757,.T.);
#2618=EDGE_CURVE('',#2117,#2118,#576,.T.);
#2619=EDGE_CURVE('',#2119,#2118,#1758,.T.);
#2620=EDGE_CURVE('',#2119,#2080,#577,.T.);
#2621=EDGE_CURVE('',#2079,#2120,#578,.T.);
#2622=EDGE_CURVE('',#2121,#2120,#1759,.T.);
#2623=EDGE_CURVE('',#2121,#2109,#579,.T.);
#2624=EDGE_CURVE('',#2122,#2123,#580,.T.);
#2625=EDGE_CURVE('',#2123,#2060,#581,.T.);
#2626=EDGE_CURVE('',#2059,#2122,#582,.T.);
#2627=EDGE_CURVE('',#2096,#2111,#1760,.T.);
#2628=EDGE_CURVE('',#2113,#2107,#583,.T.);
#2629=EDGE_CURVE('',#2112,#2108,#584,.T.);
#2630=EDGE_CURVE('',#2093,#2088,#585,.T.);
#2631=EDGE_CURVE('',#2092,#2089,#586,.T.);
#2632=EDGE_CURVE('',#2124,#2125,#587,.T.);
#2633=EDGE_CURVE('',#2125,#2126,#588,.T.);
#2634=EDGE_CURVE('',#2126,#2127,#589,.T.);
#2635=EDGE_CURVE('',#2127,#2124,#590,.T.);
#2636=EDGE_CURVE('',#2128,#2051,#591,.T.);
#2637=EDGE_CURVE('',#2050,#2129,#592,.T.);
#2638=EDGE_CURVE('',#2129,#2130,#1761,.T.);
#2639=EDGE_CURVE('',#2130,#2131,#593,.T.);
#2640=EDGE_CURVE('',#2131,#2132,#594,.T.);
#2641=EDGE_CURVE('',#2132,#2133,#595,.T.);
#2642=EDGE_CURVE('',#2133,#2128,#1762,.T.);
#2643=EDGE_CURVE('',#2134,#2135,#1763,.T.);
#2644=EDGE_CURVE('',#2135,#2136,#596,.T.);
#2645=EDGE_CURVE('',#2136,#2137,#597,.T.);
#2646=EDGE_CURVE('',#2137,#2134,#598,.T.);
#2647=EDGE_CURVE('',#2105,#2115,#1764,.T.);
#2648=EDGE_CURVE('',#2106,#2114,#1765,.T.);
#2649=EDGE_CURVE('',#2138,#2139,#599,.T.);
#2650=EDGE_CURVE('',#2139,#2140,#600,.T.);
#2651=EDGE_CURVE('',#2140,#2141,#601,.T.);
#2652=EDGE_CURVE('',#2141,#2138,#602,.T.);
#2653=EDGE_CURVE('',#2136,#2139,#1766,.T.);
#2654=EDGE_CURVE('',#2138,#2137,#1767,.T.);
#2655=EDGE_CURVE('',#2122,#2125,#1768,.T.);
#2656=EDGE_CURVE('',#2124,#2123,#1769,.T.);
#2657=EDGE_CURVE('',#2122,#2110,#1770,.T.);
#2658=EDGE_CURVE('',#2097,#2123,#1771,.T.);
#2659=EDGE_CURVE('',#2125,#2109,#1772,.T.);
#2660=EDGE_CURVE('',#2098,#2124,#1773,.T.);
#2661=EDGE_CURVE('',#2126,#2121,#1774,.T.);
#2662=EDGE_CURVE('',#2127,#2086,#1775,.T.);
#2663=EDGE_CURVE('',#2087,#2126,#1776,.T.);
#2664=EDGE_CURVE('',#2099,#2127,#1777,.T.);
#2665=EDGE_CURVE('',#2087,#2120,#1778,.T.);
#2666=EDGE_CURVE('',#2100,#2086,#1779,.T.);
#2667=EDGE_CURVE('',#2055,#2079,#21,.T.);
#2668=EDGE_CURVE('',#2094,#2085,#1780,.T.);
#2669=EDGE_CURVE('',#2090,#2084,#1781,.T.);
#2670=EDGE_CURVE('',#2067,#2083,#1782,.T.);
#2671=EDGE_CURVE('',#2054,#2076,#22,.T.);
#2672=EDGE_CURVE('',#2068,#2082,#1783,.T.);
#2673=EDGE_CURVE('',#2135,#2105,#1784,.T.);
#2674=EDGE_CURVE('',#2115,#2134,#1785,.T.);
#2675=EDGE_CURVE('',#2116,#2137,#1786,.T.);
#2676=EDGE_CURVE('',#2136,#2104,#1787,.T.);
#2677=EDGE_CURVE('',#2117,#2138,#1788,.T.);
#2678=EDGE_CURVE('',#2139,#2103,#1789,.T.);
#2679=EDGE_CURVE('',#2118,#2141,#1790,.T.);
#2680=EDGE_CURVE('',#2140,#2102,#1791,.T.);
#2681=EDGE_CURVE('',#2141,#2131,#1792,.T.);
#2682=EDGE_CURVE('',#2132,#2140,#1793,.T.);
#2683=EDGE_CURVE('',#2119,#2131,#1794,.T.);
#2684=EDGE_CURVE('',#2132,#2101,#1795,.T.);
#2685=EDGE_CURVE('',#2080,#2130,#23,.T.);
#2686=EDGE_CURVE('',#2133,#2095,#1796,.T.);
#2687=EDGE_CURVE('',#2081,#2130,#1797,.T.);
#2688=EDGE_CURVE('',#2128,#2091,#1798,.T.);
#2689=EDGE_CURVE('',#2073,#2129,#1799,.T.);
#2690=EDGE_CURVE('',#2075,#2129,#24,.T.);
#2691=EDGE_CURVE('',#2142,#2142,#1800,.T.);
#2692=EDGE_CURVE('',#2142,#2143,#603,.T.);
#2693=EDGE_CURVE('',#2143,#2143,#1801,.T.);
#2694=EDGE_CURVE('',#2144,#2144,#1802,.T.);
#2695=EDGE_CURVE('',#2144,#2145,#604,.T.);
#2696=EDGE_CURVE('',#2145,#2145,#1803,.T.);
#2697=EDGE_CURVE('',#2146,#2147,#1804,.T.);
#2698=EDGE_CURVE('',#2146,#2148,#605,.T.);
#2699=EDGE_CURVE('',#2148,#2149,#1805,.T.);
#2700=EDGE_CURVE('',#2147,#2149,#606,.T.);
#2701=EDGE_CURVE('',#2147,#2150,#607,.T.);
#2702=EDGE_CURVE('',#2150,#2151,#1806,.T.);
#2703=EDGE_CURVE('',#2151,#2146,#608,.T.);
#2704=EDGE_CURVE('',#2152,#2148,#609,.T.);
#2705=EDGE_CURVE('',#2153,#2152,#1807,.T.);
#2706=EDGE_CURVE('',#2149,#2153,#610,.T.);
#2707=EDGE_CURVE('',#2150,#2153,#611,.T.);
#2708=EDGE_CURVE('',#2151,#2152,#612,.T.);
#2709=EDGE_CURVE('',#2154,#2155,#1808,.T.);
#2710=EDGE_CURVE('',#2155,#2154,#1809,.T.);
#2711=EDGE_CURVE('',#2155,#2156,#613,.T.);
#2712=EDGE_CURVE('',#2156,#2156,#1810,.T.);
#2713=EDGE_CURVE('',#2157,#2158,#1811,.T.);
#2714=EDGE_CURVE('',#2158,#2157,#1812,.T.);
#2715=EDGE_CURVE('',#2158,#2159,#614,.T.);
#2716=EDGE_CURVE('',#2159,#2159,#1813,.T.);
#2717=EDGE_CURVE('',#2160,#2160,#1814,.T.);
#2718=EDGE_CURVE('',#2160,#2161,#615,.T.);
#2719=EDGE_CURVE('',#2161,#2161,#1815,.T.);
#2720=EDGE_CURVE('',#2162,#2162,#1816,.T.);
#2721=EDGE_CURVE('',#2162,#2163,#616,.T.);
#2722=EDGE_CURVE('',#2163,#2163,#1817,.T.);
#2723=EDGE_CURVE('',#2164,#2164,#1818,.T.);
#2724=EDGE_CURVE('',#2164,#2162,#617,.T.);
#2725=EDGE_CURVE('',#2157,#2165,#618,.T.);
#2726=EDGE_CURVE('',#2165,#2165,#1819,.T.);
#2727=EDGE_CURVE('',#2166,#2166,#1820,.T.);
#2728=EDGE_CURVE('',#2166,#2160,#619,.T.);
#2729=EDGE_CURVE('',#2154,#2167,#620,.T.);
#2730=EDGE_CURVE('',#2167,#2167,#1821,.T.);
#2731=EDGE_CURVE('',#2168,#2169,#621,.T.);
#2732=EDGE_CURVE('',#2169,#2170,#622,.T.);
#2733=EDGE_CURVE('',#2170,#2171,#623,.T.);
#2734=EDGE_CURVE('',#2171,#2172,#624,.T.);
#2735=EDGE_CURVE('',#2172,#2173,#625,.T.);
#2736=EDGE_CURVE('',#2173,#2174,#626,.T.);
#2737=EDGE_CURVE('',#2174,#2175,#627,.T.);
#2738=EDGE_CURVE('',#2175,#2176,#628,.T.);
#2739=EDGE_CURVE('',#2176,#2168,#629,.T.);
#2740=EDGE_CURVE('',#2177,#2178,#630,.T.);
#2741=EDGE_CURVE('',#2179,#2177,#631,.T.);
#2742=EDGE_CURVE('',#2180,#2179,#632,.T.);
#2743=EDGE_CURVE('',#2181,#2180,#633,.T.);
#2744=EDGE_CURVE('',#2182,#2181,#634,.T.);
#2745=EDGE_CURVE('',#2183,#2182,#635,.T.);
#2746=EDGE_CURVE('',#2184,#2183,#636,.T.);
#2747=EDGE_CURVE('',#2185,#2184,#637,.T.);
#2748=EDGE_CURVE('',#2178,#2185,#638,.T.);
#2749=EDGE_CURVE('',#2169,#2178,#639,.T.);
#2750=EDGE_CURVE('',#2168,#2177,#640,.T.);
#2751=EDGE_CURVE('',#2170,#2185,#641,.T.);
#2752=EDGE_CURVE('',#2171,#2184,#642,.T.);
#2753=EDGE_CURVE('',#2172,#2183,#643,.T.);
#2754=EDGE_CURVE('',#2173,#2182,#644,.T.);
#2755=EDGE_CURVE('',#2174,#2181,#645,.T.);
#2756=EDGE_CURVE('',#2175,#2180,#646,.T.);
#2757=EDGE_CURVE('',#2176,#2179,#647,.T.);
#2758=ORIENTED_EDGE('',*,*,#2186,.T.);
#2759=ORIENTED_EDGE('',*,*,#2187,.T.);
#2760=ORIENTED_EDGE('',*,*,#2188,.T.);
#2761=ORIENTED_EDGE('',*,*,#2189,.F.);
#2762=ORIENTED_EDGE('',*,*,#2190,.F.);
#2763=ORIENTED_EDGE('',*,*,#2191,.T.);
#2764=ORIENTED_EDGE('',*,*,#2192,.F.);
#2765=ORIENTED_EDGE('',*,*,#2191,.F.);
#2766=ORIENTED_EDGE('',*,*,#2193,.F.);
#2767=ORIENTED_EDGE('',*,*,#2194,.T.);
#2768=ORIENTED_EDGE('',*,*,#2190,.T.);
#2769=ORIENTED_EDGE('',*,*,#2194,.F.);
#2770=ORIENTED_EDGE('',*,*,#2195,.F.);
#2771=ORIENTED_EDGE('',*,*,#2196,.T.);
#2772=ORIENTED_EDGE('',*,*,#2197,.F.);
#2773=ORIENTED_EDGE('',*,*,#2196,.F.);
#2774=ORIENTED_EDGE('',*,*,#2198,.T.);
#2775=ORIENTED_EDGE('',*,*,#2199,.T.);
#2776=ORIENTED_EDGE('',*,*,#2195,.T.);
#2777=ORIENTED_EDGE('',*,*,#2199,.F.);
#2778=ORIENTED_EDGE('',*,*,#2200,.T.);
#2779=ORIENTED_EDGE('',*,*,#2201,.F.);
#2780=ORIENTED_EDGE('',*,*,#2202,.F.);
#2781=ORIENTED_EDGE('',*,*,#2203,.F.);
#2782=ORIENTED_EDGE('',*,*,#2204,.T.);
#2783=ORIENTED_EDGE('',*,*,#2205,.T.);
#2784=ORIENTED_EDGE('',*,*,#2206,.F.);
#2785=ORIENTED_EDGE('',*,*,#2205,.F.);
#2786=ORIENTED_EDGE('',*,*,#2207,.T.);
#2787=ORIENTED_EDGE('',*,*,#2208,.T.);
#2788=ORIENTED_EDGE('',*,*,#2209,.F.);
#2789=ORIENTED_EDGE('',*,*,#2208,.F.);
#2790=ORIENTED_EDGE('',*,*,#2210,.F.);
#2791=ORIENTED_EDGE('',*,*,#2211,.T.);
#2792=ORIENTED_EDGE('',*,*,#2212,.T.);
#2793=ORIENTED_EDGE('',*,*,#2213,.T.);
#2794=ORIENTED_EDGE('',*,*,#2214,.F.);
#2795=ORIENTED_EDGE('',*,*,#2215,.T.);
#2796=ORIENTED_EDGE('',*,*,#2216,.T.);
#2797=ORIENTED_EDGE('',*,*,#2217,.T.);
#2798=ORIENTED_EDGE('',*,*,#2218,.F.);
#2799=ORIENTED_EDGE('',*,*,#2219,.T.);
#2800=ORIENTED_EDGE('',*,*,#2220,.T.);
#2801=ORIENTED_EDGE('',*,*,#2221,.T.);
#2802=ORIENTED_EDGE('',*,*,#2222,.T.);
#2803=ORIENTED_EDGE('',*,*,#2223,.T.);
#2804=ORIENTED_EDGE('',*,*,#2224,.F.);
#2805=ORIENTED_EDGE('',*,*,#2225,.T.);
#2806=ORIENTED_EDGE('',*,*,#2226,.T.);
#2807=ORIENTED_EDGE('',*,*,#2227,.T.);
#2808=ORIENTED_EDGE('',*,*,#2187,.F.);
#2809=ORIENTED_EDGE('',*,*,#2228,.T.);
#2810=ORIENTED_EDGE('',*,*,#2189,.T.);
#2811=ORIENTED_EDGE('',*,*,#2229,.T.);
#2812=ORIENTED_EDGE('',*,*,#2230,.F.);
#2813=ORIENTED_EDGE('',*,*,#2231,.T.);
#2814=ORIENTED_EDGE('',*,*,#2232,.F.);
#2815=ORIENTED_EDGE('',*,*,#2233,.F.);
#2816=ORIENTED_EDGE('',*,*,#2234,.T.);
#2817=ORIENTED_EDGE('',*,*,#2235,.T.);
#2818=ORIENTED_EDGE('',*,*,#2236,.T.);
#2819=ORIENTED_EDGE('',*,*,#2237,.T.);
#2820=ORIENTED_EDGE('',*,*,#2238,.T.);
#2821=ORIENTED_EDGE('',*,*,#2239,.T.);
#2822=ORIENTED_EDGE('',*,*,#2240,.T.);
#2823=ORIENTED_EDGE('',*,*,#2241,.F.);
#2824=ORIENTED_EDGE('',*,*,#2242,.T.);
#2825=ORIENTED_EDGE('',*,*,#2243,.T.);
#2826=ORIENTED_EDGE('',*,*,#2244,.T.);
#2827=ORIENTED_EDGE('',*,*,#2245,.F.);
#2828=ORIENTED_EDGE('',*,*,#2246,.F.);
#2829=ORIENTED_EDGE('',*,*,#2247,.T.);
#2830=ORIENTED_EDGE('',*,*,#2248,.T.);
#2831=ORIENTED_EDGE('',*,*,#2249,.T.);
#2832=ORIENTED_EDGE('',*,*,#2250,.T.);
#2833=ORIENTED_EDGE('',*,*,#2251,.T.);
#2834=ORIENTED_EDGE('',*,*,#2252,.T.);
#2835=ORIENTED_EDGE('',*,*,#2253,.T.);
#2836=ORIENTED_EDGE('',*,*,#2193,.T.);
#2837=ORIENTED_EDGE('',*,*,#2198,.F.);
#2838=ORIENTED_EDGE('',*,*,#2207,.F.);
#2839=ORIENTED_EDGE('',*,*,#2204,.F.);
#2840=ORIENTED_EDGE('',*,*,#2254,.F.);
#2841=ORIENTED_EDGE('',*,*,#2229,.F.);
#2842=ORIENTED_EDGE('',*,*,#2188,.F.);
#2843=ORIENTED_EDGE('',*,*,#2227,.F.);
#2844=ORIENTED_EDGE('',*,*,#2255,.F.);
#2845=ORIENTED_EDGE('',*,*,#2223,.F.);
#2846=ORIENTED_EDGE('',*,*,#2256,.F.);
#2847=ORIENTED_EDGE('',*,*,#2221,.F.);
#2848=ORIENTED_EDGE('',*,*,#2257,.F.);
#2849=ORIENTED_EDGE('',*,*,#2217,.F.);
#2850=ORIENTED_EDGE('',*,*,#2258,.F.);
#2851=ORIENTED_EDGE('',*,*,#2213,.F.);
#2852=ORIENTED_EDGE('',*,*,#2259,.F.);
#2853=ORIENTED_EDGE('',*,*,#2260,.T.);
#2854=ORIENTED_EDGE('',*,*,#2261,.F.);
#2855=ORIENTED_EDGE('',*,*,#2262,.F.);
#2856=ORIENTED_EDGE('',*,*,#2263,.T.);
#2857=ORIENTED_EDGE('',*,*,#2264,.T.);
#2858=ORIENTED_EDGE('',*,*,#2265,.T.);
#2859=ORIENTED_EDGE('',*,*,#2233,.T.);
#2860=ORIENTED_EDGE('',*,*,#2266,.T.);
#2861=ORIENTED_EDGE('',*,*,#2267,.T.);
#2862=ORIENTED_EDGE('',*,*,#2268,.F.);
#2863=ORIENTED_EDGE('',*,*,#2253,.F.);
#2864=ORIENTED_EDGE('',*,*,#2269,.T.);
#2865=ORIENTED_EDGE('',*,*,#2222,.F.);
#2866=ORIENTED_EDGE('',*,*,#2270,.T.);
#2867=ORIENTED_EDGE('',*,*,#2218,.T.);
#2868=ORIENTED_EDGE('',*,*,#2256,.T.);
#2869=ORIENTED_EDGE('',*,*,#2271,.T.);
#2870=ORIENTED_EDGE('',*,*,#2272,.T.);
#2871=ORIENTED_EDGE('',*,*,#2273,.F.);
#2872=ORIENTED_EDGE('',*,*,#2244,.F.);
#2873=ORIENTED_EDGE('',*,*,#2274,.T.);
#2874=ORIENTED_EDGE('',*,*,#2275,.F.);
#2875=ORIENTED_EDGE('',*,*,#2276,.F.);
#2876=ORIENTED_EDGE('',*,*,#2240,.F.);
#2877=ORIENTED_EDGE('',*,*,#2277,.T.);
#2878=ORIENTED_EDGE('',*,*,#2278,.T.);
#2879=ORIENTED_EDGE('',*,*,#2279,.F.);
#2880=ORIENTED_EDGE('',*,*,#2248,.F.);
#2881=ORIENTED_EDGE('',*,*,#2280,.T.);
#2882=ORIENTED_EDGE('',*,*,#2259,.T.);
#2883=ORIENTED_EDGE('',*,*,#2212,.F.);
#2884=ORIENTED_EDGE('',*,*,#2281,.T.);
#2885=ORIENTED_EDGE('',*,*,#2280,.F.);
#2886=ORIENTED_EDGE('',*,*,#2282,.T.);
#2887=ORIENTED_EDGE('',*,*,#2230,.T.);
#2888=ORIENTED_EDGE('',*,*,#2254,.T.);
#2889=ORIENTED_EDGE('',*,*,#2224,.T.);
#2890=ORIENTED_EDGE('',*,*,#2255,.T.);
#2891=ORIENTED_EDGE('',*,*,#2226,.F.);
#2892=ORIENTED_EDGE('',*,*,#2283,.T.);
#2893=ORIENTED_EDGE('',*,*,#2214,.T.);
#2894=ORIENTED_EDGE('',*,*,#2257,.T.);
#2895=ORIENTED_EDGE('',*,*,#2220,.F.);
#2896=ORIENTED_EDGE('',*,*,#2284,.T.);
#2897=ORIENTED_EDGE('',*,*,#2210,.T.);
#2898=ORIENTED_EDGE('',*,*,#2258,.T.);
#2899=ORIENTED_EDGE('',*,*,#2216,.F.);
#2900=ORIENTED_EDGE('',*,*,#2285,.T.);
#2901=ORIENTED_EDGE('',*,*,#2260,.F.);
#2902=ORIENTED_EDGE('',*,*,#2286,.T.);
#2903=ORIENTED_EDGE('',*,*,#2267,.F.);
#2904=ORIENTED_EDGE('',*,*,#2287,.F.);
#2905=ORIENTED_EDGE('',*,*,#2288,.F.);
#2906=ORIENTED_EDGE('',*,*,#2289,.F.);
#2907=ORIENTED_EDGE('',*,*,#2290,.F.);
#2908=ORIENTED_EDGE('',*,*,#2278,.F.);
#2909=ORIENTED_EDGE('',*,*,#2291,.F.);
#2910=ORIENTED_EDGE('',*,*,#2292,.F.);
#2911=ORIENTED_EDGE('',*,*,#2293,.F.);
#2912=ORIENTED_EDGE('',*,*,#2294,.F.);
#2913=ORIENTED_EDGE('',*,*,#2295,.F.);
#2914=ORIENTED_EDGE('',*,*,#2296,.T.);
#2915=ORIENTED_EDGE('',*,*,#2264,.F.);
#2916=ORIENTED_EDGE('',*,*,#2297,.F.);
#2917=ORIENTED_EDGE('',*,*,#2206,.T.);
#2918=ORIENTED_EDGE('',*,*,#2209,.T.);
#2919=ORIENTED_EDGE('',*,*,#2290,.T.);
#2920=ORIENTED_EDGE('',*,*,#2298,.F.);
#2921=ORIENTED_EDGE('',*,*,#2249,.F.);
#2922=ORIENTED_EDGE('',*,*,#2279,.T.);
#2923=ORIENTED_EDGE('',*,*,#2289,.T.);
#2924=ORIENTED_EDGE('',*,*,#2299,.F.);
#2925=ORIENTED_EDGE('',*,*,#2250,.F.);
#2926=ORIENTED_EDGE('',*,*,#2298,.T.);
#2927=ORIENTED_EDGE('',*,*,#2288,.T.);
#2928=ORIENTED_EDGE('',*,*,#2300,.F.);
#2929=ORIENTED_EDGE('',*,*,#2251,.F.);
#2930=ORIENTED_EDGE('',*,*,#2299,.T.);
#2931=ORIENTED_EDGE('',*,*,#2287,.T.);
#2932=ORIENTED_EDGE('',*,*,#2269,.F.);
#2933=ORIENTED_EDGE('',*,*,#2252,.F.);
#2934=ORIENTED_EDGE('',*,*,#2300,.T.);
#2935=ORIENTED_EDGE('',*,*,#2235,.F.);
#2936=ORIENTED_EDGE('',*,*,#2301,.F.);
#2937=ORIENTED_EDGE('',*,*,#2295,.T.);
#2938=ORIENTED_EDGE('',*,*,#2302,.F.);
#2939=ORIENTED_EDGE('',*,*,#2294,.T.);
#2940=ORIENTED_EDGE('',*,*,#2303,.F.);
#2941=ORIENTED_EDGE('',*,*,#2236,.F.);
#2942=ORIENTED_EDGE('',*,*,#2302,.T.);
#2943=ORIENTED_EDGE('',*,*,#2293,.T.);
#2944=ORIENTED_EDGE('',*,*,#2304,.F.);
#2945=ORIENTED_EDGE('',*,*,#2237,.F.);
#2946=ORIENTED_EDGE('',*,*,#2303,.T.);
#2947=ORIENTED_EDGE('',*,*,#2292,.T.);
#2948=ORIENTED_EDGE('',*,*,#2305,.F.);
#2949=ORIENTED_EDGE('',*,*,#2238,.F.);
#2950=ORIENTED_EDGE('',*,*,#2304,.T.);
#2951=ORIENTED_EDGE('',*,*,#2291,.T.);
#2952=ORIENTED_EDGE('',*,*,#2277,.F.);
#2953=ORIENTED_EDGE('',*,*,#2239,.F.);
#2954=ORIENTED_EDGE('',*,*,#2305,.T.);
#2955=ORIENTED_EDGE('',*,*,#2306,.T.);
#2956=ORIENTED_EDGE('',*,*,#2242,.F.);
#2957=ORIENTED_EDGE('',*,*,#2307,.F.);
#2958=ORIENTED_EDGE('',*,*,#2275,.T.);
#2959=ORIENTED_EDGE('',*,*,#2276,.T.);
#2960=ORIENTED_EDGE('',*,*,#2307,.T.);
#2961=ORIENTED_EDGE('',*,*,#2241,.T.);
#2962=ORIENTED_EDGE('',*,*,#2274,.F.);
#2963=ORIENTED_EDGE('',*,*,#2243,.F.);
#2964=ORIENTED_EDGE('',*,*,#2306,.F.);
#2965=ORIENTED_EDGE('',*,*,#2308,.F.);
#2966=ORIENTED_EDGE('',*,*,#2272,.F.);
#2967=ORIENTED_EDGE('',*,*,#2309,.T.);
#2968=ORIENTED_EDGE('',*,*,#2246,.T.);
#2969=ORIENTED_EDGE('',*,*,#2271,.F.);
#2970=ORIENTED_EDGE('',*,*,#2247,.F.);
#2971=ORIENTED_EDGE('',*,*,#2309,.F.);
#2972=ORIENTED_EDGE('',*,*,#2273,.T.);
#2973=ORIENTED_EDGE('',*,*,#2308,.T.);
#2974=ORIENTED_EDGE('',*,*,#2245,.T.);
#2975=ORIENTED_EDGE('',*,*,#2266,.F.);
#2976=ORIENTED_EDGE('',*,*,#2232,.T.);
#2977=ORIENTED_EDGE('',*,*,#2268,.T.);
#2978=ORIENTED_EDGE('',*,*,#2286,.F.);
#2979=ORIENTED_EDGE('',*,*,#2301,.T.);
#2980=ORIENTED_EDGE('',*,*,#2234,.F.);
#2981=ORIENTED_EDGE('',*,*,#2265,.F.);
#2982=ORIENTED_EDGE('',*,*,#2296,.F.);
#2983=ORIENTED_EDGE('',*,*,#2310,.F.);
#2984=ORIENTED_EDGE('',*,*,#2311,.T.);
#2985=ORIENTED_EDGE('',*,*,#2202,.T.);
#2986=ORIENTED_EDGE('',*,*,#2312,.T.);
#2987=ORIENTED_EDGE('',*,*,#2313,.F.);
#2988=ORIENTED_EDGE('',*,*,#2297,.T.);
#2989=ORIENTED_EDGE('',*,*,#2314,.F.);
#2990=ORIENTED_EDGE('',*,*,#2315,.T.);
#2991=ORIENTED_EDGE('',*,*,#2316,.T.);
#2992=ORIENTED_EDGE('',*,*,#2317,.T.);
#2993=ORIENTED_EDGE('',*,*,#2318,.F.);
#2994=ORIENTED_EDGE('',*,*,#2200,.F.);
#2995=ORIENTED_EDGE('',*,*,#2262,.T.);
#2996=ORIENTED_EDGE('',*,*,#2319,.F.);
#2997=ORIENTED_EDGE('',*,*,#2316,.F.);
#2998=ORIENTED_EDGE('',*,*,#2320,.T.);
#2999=ORIENTED_EDGE('',*,*,#2313,.T.);
#3000=ORIENTED_EDGE('',*,*,#2321,.T.);
#3001=ORIENTED_EDGE('',*,*,#2317,.F.);
#3002=ORIENTED_EDGE('',*,*,#2319,.T.);
#3003=ORIENTED_EDGE('',*,*,#2261,.T.);
#3004=ORIENTED_EDGE('',*,*,#2315,.F.);
#3005=ORIENTED_EDGE('',*,*,#2322,.T.);
#3006=ORIENTED_EDGE('',*,*,#2310,.T.);
#3007=ORIENTED_EDGE('',*,*,#2263,.F.);
#3008=ORIENTED_EDGE('',*,*,#2320,.F.);
#3009=ORIENTED_EDGE('',*,*,#2322,.F.);
#3010=ORIENTED_EDGE('',*,*,#2314,.T.);
#3011=ORIENTED_EDGE('',*,*,#2203,.T.);
#3012=ORIENTED_EDGE('',*,*,#2311,.F.);
#3013=ORIENTED_EDGE('',*,*,#2282,.F.);
#3014=ORIENTED_EDGE('',*,*,#2281,.F.);
#3015=ORIENTED_EDGE('',*,*,#2211,.F.);
#3016=ORIENTED_EDGE('',*,*,#2285,.F.);
#3017=ORIENTED_EDGE('',*,*,#2215,.F.);
#3018=ORIENTED_EDGE('',*,*,#2284,.F.);
#3019=ORIENTED_EDGE('',*,*,#2219,.F.);
#3020=ORIENTED_EDGE('',*,*,#2270,.F.);
#3021=ORIENTED_EDGE('',*,*,#2225,.F.);
#3022=ORIENTED_EDGE('',*,*,#2283,.F.);
#3023=ORIENTED_EDGE('',*,*,#2228,.F.);
#3024=ORIENTED_EDGE('',*,*,#2186,.F.);
#3025=ORIENTED_EDGE('',*,*,#2231,.F.);
#3026=ORIENTED_EDGE('',*,*,#2321,.F.);
#3027=ORIENTED_EDGE('',*,*,#2312,.F.);
#3028=ORIENTED_EDGE('',*,*,#2201,.T.);
#3029=ORIENTED_EDGE('',*,*,#2318,.T.);
#3030=ORIENTED_EDGE('',*,*,#2197,.T.);
#3031=ORIENTED_EDGE('',*,*,#2192,.T.);
#3032=ORIENTED_EDGE('',*,*,#2323,.T.);
#3033=ORIENTED_EDGE('',*,*,#2324,.T.);
#3034=ORIENTED_EDGE('',*,*,#2325,.T.);
#3035=ORIENTED_EDGE('',*,*,#2324,.F.);
#3036=ORIENTED_EDGE('',*,*,#2326,.F.);
#3037=ORIENTED_EDGE('',*,*,#2327,.T.);
#3038=ORIENTED_EDGE('',*,*,#2328,.T.);
#3039=ORIENTED_EDGE('',*,*,#2327,.F.);
#3040=ORIENTED_EDGE('',*,*,#2329,.F.);
#3041=ORIENTED_EDGE('',*,*,#2330,.T.);
#3042=ORIENTED_EDGE('',*,*,#2331,.F.);
#3043=ORIENTED_EDGE('',*,*,#2332,.F.);
#3044=ORIENTED_EDGE('',*,*,#2333,.F.);
#3045=ORIENTED_EDGE('',*,*,#2334,.F.);
#3046=ORIENTED_EDGE('',*,*,#2335,.T.);
#3047=ORIENTED_EDGE('',*,*,#2336,.F.);
#3048=ORIENTED_EDGE('',*,*,#2337,.F.);
#3049=ORIENTED_EDGE('',*,*,#2330,.F.);
#3050=ORIENTED_EDGE('',*,*,#2338,.F.);
#3051=ORIENTED_EDGE('',*,*,#2339,.T.);
#3052=ORIENTED_EDGE('',*,*,#2340,.T.);
#3053=ORIENTED_EDGE('',*,*,#2339,.F.);
#3054=ORIENTED_EDGE('',*,*,#2338,.T.);
#3055=ORIENTED_EDGE('',*,*,#2341,.F.);
#3056=ORIENTED_EDGE('',*,*,#2342,.F.);
#3057=ORIENTED_EDGE('',*,*,#2343,.F.);
#3058=ORIENTED_EDGE('',*,*,#2344,.F.);
#3059=ORIENTED_EDGE('',*,*,#2345,.F.);
#3060=ORIENTED_EDGE('',*,*,#2346,.F.);
#3061=ORIENTED_EDGE('',*,*,#2340,.F.);
#3062=ORIENTED_EDGE('',*,*,#2329,.T.);
#3063=ORIENTED_EDGE('',*,*,#2342,.T.);
#3064=ORIENTED_EDGE('',*,*,#2347,.F.);
#3065=ORIENTED_EDGE('',*,*,#2348,.F.);
#3066=ORIENTED_EDGE('',*,*,#2349,.T.);
#3067=ORIENTED_EDGE('',*,*,#2343,.T.);
#3068=ORIENTED_EDGE('',*,*,#2349,.F.);
#3069=ORIENTED_EDGE('',*,*,#2350,.F.);
#3070=ORIENTED_EDGE('',*,*,#2351,.T.);
#3071=ORIENTED_EDGE('',*,*,#2344,.T.);
#3072=ORIENTED_EDGE('',*,*,#2351,.F.);
#3073=ORIENTED_EDGE('',*,*,#2352,.F.);
#3074=ORIENTED_EDGE('',*,*,#2353,.T.);
#3075=ORIENTED_EDGE('',*,*,#2345,.T.);
#3076=ORIENTED_EDGE('',*,*,#2353,.F.);
#3077=ORIENTED_EDGE('',*,*,#2354,.F.);
#3078=ORIENTED_EDGE('',*,*,#2355,.T.);
#3079=ORIENTED_EDGE('',*,*,#2346,.T.);
#3080=ORIENTED_EDGE('',*,*,#2355,.F.);
#3081=ORIENTED_EDGE('',*,*,#2356,.F.);
#3082=ORIENTED_EDGE('',*,*,#2357,.T.);
#3083=ORIENTED_EDGE('',*,*,#2341,.T.);
#3084=ORIENTED_EDGE('',*,*,#2357,.F.);
#3085=ORIENTED_EDGE('',*,*,#2358,.F.);
#3086=ORIENTED_EDGE('',*,*,#2347,.T.);
#3087=ORIENTED_EDGE('',*,*,#2348,.T.);
#3088=ORIENTED_EDGE('',*,*,#2358,.T.);
#3089=ORIENTED_EDGE('',*,*,#2356,.T.);
#3090=ORIENTED_EDGE('',*,*,#2354,.T.);
#3091=ORIENTED_EDGE('',*,*,#2352,.T.);
#3092=ORIENTED_EDGE('',*,*,#2350,.T.);
#3093=ORIENTED_EDGE('',*,*,#2359,.T.);
#3094=ORIENTED_EDGE('',*,*,#2360,.T.);
#3095=ORIENTED_EDGE('',*,*,#2361,.T.);
#3096=ORIENTED_EDGE('',*,*,#2362,.T.);
#3097=ORIENTED_EDGE('',*,*,#2363,.T.);
#3098=ORIENTED_EDGE('',*,*,#2364,.T.);
#3099=ORIENTED_EDGE('',*,*,#2323,.F.);
#3100=ORIENTED_EDGE('',*,*,#2365,.F.);
#3101=ORIENTED_EDGE('',*,*,#2336,.T.);
#3102=ORIENTED_EDGE('',*,*,#2366,.F.);
#3103=ORIENTED_EDGE('',*,*,#2367,.F.);
#3104=ORIENTED_EDGE('',*,*,#2335,.F.);
#3105=ORIENTED_EDGE('',*,*,#2368,.F.);
#3106=ORIENTED_EDGE('',*,*,#2369,.F.);
#3107=ORIENTED_EDGE('',*,*,#2334,.T.);
#3108=ORIENTED_EDGE('',*,*,#2370,.F.);
#3109=ORIENTED_EDGE('',*,*,#2371,.F.);
#3110=ORIENTED_EDGE('',*,*,#2333,.T.);
#3111=ORIENTED_EDGE('',*,*,#2372,.F.);
#3112=ORIENTED_EDGE('',*,*,#2373,.F.);
#3113=ORIENTED_EDGE('',*,*,#2332,.T.);
#3114=ORIENTED_EDGE('',*,*,#2374,.F.);
#3115=ORIENTED_EDGE('',*,*,#2375,.F.);
#3116=ORIENTED_EDGE('',*,*,#2331,.T.);
#3117=ORIENTED_EDGE('',*,*,#2337,.T.);
#3118=ORIENTED_EDGE('',*,*,#2376,.F.);
#3119=ORIENTED_EDGE('',*,*,#2372,.T.);
#3120=ORIENTED_EDGE('',*,*,#2373,.T.);
#3121=ORIENTED_EDGE('',*,*,#2377,.F.);
#3122=ORIENTED_EDGE('',*,*,#2359,.F.);
#3123=ORIENTED_EDGE('',*,*,#2378,.T.);
#3124=ORIENTED_EDGE('',*,*,#2374,.T.);
#3125=ORIENTED_EDGE('',*,*,#2375,.T.);
#3126=ORIENTED_EDGE('',*,*,#2379,.F.);
#3127=ORIENTED_EDGE('',*,*,#2360,.F.);
#3128=ORIENTED_EDGE('',*,*,#2377,.T.);
#3129=ORIENTED_EDGE('',*,*,#2376,.T.);
#3130=ORIENTED_EDGE('',*,*,#2365,.T.);
#3131=ORIENTED_EDGE('',*,*,#2380,.F.);
#3132=ORIENTED_EDGE('',*,*,#2361,.F.);
#3133=ORIENTED_EDGE('',*,*,#2379,.T.);
#3134=ORIENTED_EDGE('',*,*,#2366,.T.);
#3135=ORIENTED_EDGE('',*,*,#2367,.T.);
#3136=ORIENTED_EDGE('',*,*,#2381,.F.);
#3137=ORIENTED_EDGE('',*,*,#2362,.F.);
#3138=ORIENTED_EDGE('',*,*,#2380,.T.);
#3139=ORIENTED_EDGE('',*,*,#2368,.T.);
#3140=ORIENTED_EDGE('',*,*,#2369,.T.);
#3141=ORIENTED_EDGE('',*,*,#2382,.F.);
#3142=ORIENTED_EDGE('',*,*,#2363,.F.);
#3143=ORIENTED_EDGE('',*,*,#2381,.T.);
#3144=ORIENTED_EDGE('',*,*,#2370,.T.);
#3145=ORIENTED_EDGE('',*,*,#2371,.T.);
#3146=ORIENTED_EDGE('',*,*,#2378,.F.);
#3147=ORIENTED_EDGE('',*,*,#2364,.F.);
#3148=ORIENTED_EDGE('',*,*,#2382,.T.);
#3149=ORIENTED_EDGE('',*,*,#2328,.F.);
#3150=ORIENTED_EDGE('',*,*,#2325,.F.);
#3151=ORIENTED_EDGE('',*,*,#2326,.T.);
#3152=ORIENTED_EDGE('',*,*,#2383,.F.);
#3153=ORIENTED_EDGE('',*,*,#2384,.T.);
#3154=ORIENTED_EDGE('',*,*,#2385,.T.);
#3155=ORIENTED_EDGE('',*,*,#2386,.F.);
#3156=ORIENTED_EDGE('',*,*,#2387,.F.);
#3157=ORIENTED_EDGE('',*,*,#2388,.T.);
#3158=ORIENTED_EDGE('',*,*,#2389,.T.);
#3159=ORIENTED_EDGE('',*,*,#2390,.F.);
#3160=ORIENTED_EDGE('',*,*,#2391,.F.);
#3161=ORIENTED_EDGE('',*,*,#2392,.T.);
#3162=ORIENTED_EDGE('',*,*,#2393,.T.);
#3163=ORIENTED_EDGE('',*,*,#2394,.F.);
#3164=ORIENTED_EDGE('',*,*,#2395,.T.);
#3165=ORIENTED_EDGE('',*,*,#2396,.T.);
#3166=ORIENTED_EDGE('',*,*,#2397,.F.);
#3167=ORIENTED_EDGE('',*,*,#2396,.F.);
#3168=ORIENTED_EDGE('',*,*,#2398,.T.);
#3169=ORIENTED_EDGE('',*,*,#2399,.T.);
#3170=ORIENTED_EDGE('',*,*,#2400,.F.);
#3171=ORIENTED_EDGE('',*,*,#2399,.F.);
#3172=ORIENTED_EDGE('',*,*,#2401,.T.);
#3173=ORIENTED_EDGE('',*,*,#2402,.T.);
#3174=ORIENTED_EDGE('',*,*,#2403,.T.);
#3175=ORIENTED_EDGE('',*,*,#2402,.F.);
#3176=ORIENTED_EDGE('',*,*,#2404,.T.);
#3177=ORIENTED_EDGE('',*,*,#2405,.T.);
#3178=ORIENTED_EDGE('',*,*,#2406,.T.);
#3179=ORIENTED_EDGE('',*,*,#2404,.F.);
#3180=ORIENTED_EDGE('',*,*,#2406,.F.);
#3181=ORIENTED_EDGE('',*,*,#2407,.T.);
#3182=ORIENTED_EDGE('',*,*,#2408,.T.);
#3183=ORIENTED_EDGE('',*,*,#2409,.T.);
#3184=ORIENTED_EDGE('',*,*,#2408,.F.);
#3185=ORIENTED_EDGE('',*,*,#2410,.T.);
#3186=ORIENTED_EDGE('',*,*,#2411,.T.);
#3187=ORIENTED_EDGE('',*,*,#2412,.T.);
#3188=ORIENTED_EDGE('',*,*,#2411,.F.);
#3189=ORIENTED_EDGE('',*,*,#2410,.F.);
#3190=ORIENTED_EDGE('',*,*,#2413,.T.);
#3191=ORIENTED_EDGE('',*,*,#2414,.T.);
#3192=ORIENTED_EDGE('',*,*,#2415,.T.);
#3193=ORIENTED_EDGE('',*,*,#2414,.F.);
#3194=ORIENTED_EDGE('',*,*,#2416,.T.);
#3195=ORIENTED_EDGE('',*,*,#2417,.T.);
#3196=ORIENTED_EDGE('',*,*,#2418,.T.);
#3197=ORIENTED_EDGE('',*,*,#2417,.F.);
#3198=ORIENTED_EDGE('',*,*,#2419,.T.);
#3199=ORIENTED_EDGE('',*,*,#2420,.T.);
#3200=ORIENTED_EDGE('',*,*,#2421,.F.);
#3201=ORIENTED_EDGE('',*,*,#2420,.F.);
#3202=ORIENTED_EDGE('',*,*,#2422,.F.);
#3203=ORIENTED_EDGE('',*,*,#2423,.F.);
#3204=ORIENTED_EDGE('',*,*,#2424,.T.);
#3205=ORIENTED_EDGE('',*,*,#2425,.F.);
#3206=ORIENTED_EDGE('',*,*,#2426,.T.);
#3207=ORIENTED_EDGE('',*,*,#2427,.T.);
#3208=ORIENTED_EDGE('',*,*,#2428,.T.);
#3209=ORIENTED_EDGE('',*,*,#2429,.T.);
#3210=ORIENTED_EDGE('',*,*,#2430,.T.);
#3211=ORIENTED_EDGE('',*,*,#2431,.T.);
#3212=ORIENTED_EDGE('',*,*,#2432,.T.);
#3213=ORIENTED_EDGE('',*,*,#2433,.T.);
#3214=ORIENTED_EDGE('',*,*,#2434,.T.);
#3215=ORIENTED_EDGE('',*,*,#2435,.T.);
#3216=ORIENTED_EDGE('',*,*,#2436,.T.);
#3217=ORIENTED_EDGE('',*,*,#2437,.F.);
#3218=ORIENTED_EDGE('',*,*,#2438,.T.);
#3219=ORIENTED_EDGE('',*,*,#2439,.T.);
#3220=ORIENTED_EDGE('',*,*,#2440,.T.);
#3221=ORIENTED_EDGE('',*,*,#2441,.F.);
#3222=ORIENTED_EDGE('',*,*,#2442,.T.);
#3223=ORIENTED_EDGE('',*,*,#2443,.T.);
#3224=ORIENTED_EDGE('',*,*,#2444,.T.);
#3225=ORIENTED_EDGE('',*,*,#2445,.T.);
#3226=ORIENTED_EDGE('',*,*,#2398,.F.);
#3227=ORIENTED_EDGE('',*,*,#2446,.F.);
#3228=ORIENTED_EDGE('',*,*,#2447,.F.);
#3229=ORIENTED_EDGE('',*,*,#2448,.F.);
#3230=ORIENTED_EDGE('',*,*,#2449,.F.);
#3231=ORIENTED_EDGE('',*,*,#2450,.F.);
#3232=ORIENTED_EDGE('',*,*,#2451,.F.);
#3233=ORIENTED_EDGE('',*,*,#2452,.T.);
#3234=ORIENTED_EDGE('',*,*,#2453,.F.);
#3235=ORIENTED_EDGE('',*,*,#2454,.F.);
#3236=ORIENTED_EDGE('',*,*,#2455,.F.);
#3237=ORIENTED_EDGE('',*,*,#2456,.T.);
#3238=ORIENTED_EDGE('',*,*,#2457,.F.);
#3239=ORIENTED_EDGE('',*,*,#2458,.F.);
#3240=ORIENTED_EDGE('',*,*,#2459,.F.);
#3241=ORIENTED_EDGE('',*,*,#2460,.F.);
#3242=ORIENTED_EDGE('',*,*,#2461,.F.);
#3243=ORIENTED_EDGE('',*,*,#2462,.F.);
#3244=ORIENTED_EDGE('',*,*,#2463,.F.);
#3245=ORIENTED_EDGE('',*,*,#2464,.F.);
#3246=ORIENTED_EDGE('',*,*,#2465,.F.);
#3247=ORIENTED_EDGE('',*,*,#2403,.F.);
#3248=ORIENTED_EDGE('',*,*,#2466,.F.);
#3249=ORIENTED_EDGE('',*,*,#2436,.F.);
#3250=ORIENTED_EDGE('',*,*,#2467,.T.);
#3251=ORIENTED_EDGE('',*,*,#2457,.T.);
#3252=ORIENTED_EDGE('',*,*,#2415,.F.);
#3253=ORIENTED_EDGE('',*,*,#2438,.F.);
#3254=ORIENTED_EDGE('',*,*,#2468,.F.);
#3255=ORIENTED_EDGE('',*,*,#2455,.T.);
#3256=ORIENTED_EDGE('',*,*,#2469,.F.);
#3257=ORIENTED_EDGE('',*,*,#2416,.F.);
#3258=ORIENTED_EDGE('',*,*,#2470,.F.);
#3259=ORIENTED_EDGE('',*,*,#2440,.F.);
#3260=ORIENTED_EDGE('',*,*,#2471,.T.);
#3261=ORIENTED_EDGE('',*,*,#2453,.T.);
#3262=ORIENTED_EDGE('',*,*,#2418,.F.);
#3263=ORIENTED_EDGE('',*,*,#2442,.F.);
#3264=ORIENTED_EDGE('',*,*,#2472,.F.);
#3265=ORIENTED_EDGE('',*,*,#2451,.T.);
#3266=ORIENTED_EDGE('',*,*,#2473,.F.);
#3267=ORIENTED_EDGE('',*,*,#2419,.F.);
#3268=ORIENTED_EDGE('',*,*,#2474,.F.);
#3269=ORIENTED_EDGE('',*,*,#2426,.F.);
#3270=ORIENTED_EDGE('',*,*,#2475,.T.);
#3271=ORIENTED_EDGE('',*,*,#2447,.T.);
#3272=ORIENTED_EDGE('',*,*,#2405,.F.);
#3273=ORIENTED_EDGE('',*,*,#2428,.F.);
#3274=ORIENTED_EDGE('',*,*,#2476,.F.);
#3275=ORIENTED_EDGE('',*,*,#2465,.T.);
#3276=ORIENTED_EDGE('',*,*,#2477,.F.);
#3277=ORIENTED_EDGE('',*,*,#2409,.F.);
#3278=ORIENTED_EDGE('',*,*,#2478,.F.);
#3279=ORIENTED_EDGE('',*,*,#2430,.F.);
#3280=ORIENTED_EDGE('',*,*,#2479,.T.);
#3281=ORIENTED_EDGE('',*,*,#2463,.T.);
#3282=ORIENTED_EDGE('',*,*,#2407,.F.);
#3283=ORIENTED_EDGE('',*,*,#2432,.F.);
#3284=ORIENTED_EDGE('',*,*,#2480,.F.);
#3285=ORIENTED_EDGE('',*,*,#2461,.T.);
#3286=ORIENTED_EDGE('',*,*,#2481,.F.);
#3287=ORIENTED_EDGE('',*,*,#2412,.F.);
#3288=ORIENTED_EDGE('',*,*,#2460,.T.);
#3289=ORIENTED_EDGE('',*,*,#2482,.F.);
#3290=ORIENTED_EDGE('',*,*,#2433,.F.);
#3291=ORIENTED_EDGE('',*,*,#2481,.T.);
#3292=ORIENTED_EDGE('',*,*,#2459,.T.);
#3293=ORIENTED_EDGE('',*,*,#2483,.F.);
#3294=ORIENTED_EDGE('',*,*,#2434,.F.);
#3295=ORIENTED_EDGE('',*,*,#2482,.T.);
#3296=ORIENTED_EDGE('',*,*,#2391,.T.);
#3297=ORIENTED_EDGE('',*,*,#2422,.T.);
#3298=ORIENTED_EDGE('',*,*,#2458,.T.);
#3299=ORIENTED_EDGE('',*,*,#2467,.F.);
#3300=ORIENTED_EDGE('',*,*,#2435,.F.);
#3301=ORIENTED_EDGE('',*,*,#2483,.T.);
#3302=ORIENTED_EDGE('',*,*,#2454,.T.);
#3303=ORIENTED_EDGE('',*,*,#2471,.F.);
#3304=ORIENTED_EDGE('',*,*,#2439,.F.);
#3305=ORIENTED_EDGE('',*,*,#2469,.T.);
#3306=ORIENTED_EDGE('',*,*,#2450,.T.);
#3307=ORIENTED_EDGE('',*,*,#2484,.F.);
#3308=ORIENTED_EDGE('',*,*,#2443,.F.);
#3309=ORIENTED_EDGE('',*,*,#2473,.T.);
#3310=ORIENTED_EDGE('',*,*,#2449,.T.);
#3311=ORIENTED_EDGE('',*,*,#2485,.F.);
#3312=ORIENTED_EDGE('',*,*,#2444,.F.);
#3313=ORIENTED_EDGE('',*,*,#2484,.T.);
#3314=ORIENTED_EDGE('',*,*,#2389,.F.);
#3315=ORIENTED_EDGE('',*,*,#2424,.F.);
#3316=ORIENTED_EDGE('',*,*,#2448,.T.);
#3317=ORIENTED_EDGE('',*,*,#2475,.F.);
#3318=ORIENTED_EDGE('',*,*,#2445,.F.);
#3319=ORIENTED_EDGE('',*,*,#2485,.T.);
#3320=ORIENTED_EDGE('',*,*,#2464,.T.);
#3321=ORIENTED_EDGE('',*,*,#2479,.F.);
#3322=ORIENTED_EDGE('',*,*,#2429,.F.);
#3323=ORIENTED_EDGE('',*,*,#2477,.T.);
#3324=ORIENTED_EDGE('',*,*,#2478,.T.);
#3325=ORIENTED_EDGE('',*,*,#2462,.T.);
#3326=ORIENTED_EDGE('',*,*,#2480,.T.);
#3327=ORIENTED_EDGE('',*,*,#2431,.F.);
#3328=ORIENTED_EDGE('',*,*,#2474,.T.);
#3329=ORIENTED_EDGE('',*,*,#2446,.T.);
#3330=ORIENTED_EDGE('',*,*,#2476,.T.);
#3331=ORIENTED_EDGE('',*,*,#2427,.F.);
#3332=ORIENTED_EDGE('',*,*,#2470,.T.);
#3333=ORIENTED_EDGE('',*,*,#2452,.F.);
#3334=ORIENTED_EDGE('',*,*,#2472,.T.);
#3335=ORIENTED_EDGE('',*,*,#2441,.T.);
#3336=ORIENTED_EDGE('',*,*,#2466,.T.);
#3337=ORIENTED_EDGE('',*,*,#2456,.F.);
#3338=ORIENTED_EDGE('',*,*,#2468,.T.);
#3339=ORIENTED_EDGE('',*,*,#2437,.T.);
#3340=ORIENTED_EDGE('',*,*,#2421,.T.);
#3341=ORIENTED_EDGE('',*,*,#2413,.F.);
#3342=ORIENTED_EDGE('',*,*,#2400,.T.);
#3343=ORIENTED_EDGE('',*,*,#2395,.F.);
#3344=ORIENTED_EDGE('',*,*,#2401,.F.);
#3345=ORIENTED_EDGE('',*,*,#2397,.T.);
#3346=ORIENTED_EDGE('',*,*,#2486,.T.);
#3347=ORIENTED_EDGE('',*,*,#2392,.F.);
#3348=ORIENTED_EDGE('',*,*,#2425,.T.);
#3349=ORIENTED_EDGE('',*,*,#2388,.F.);
#3350=ORIENTED_EDGE('',*,*,#2487,.F.);
#3351=ORIENTED_EDGE('',*,*,#2386,.T.);
#3352=ORIENTED_EDGE('',*,*,#2488,.T.);
#3353=ORIENTED_EDGE('',*,*,#2384,.F.);
#3354=ORIENTED_EDGE('',*,*,#2489,.F.);
#3355=ORIENTED_EDGE('',*,*,#2390,.T.);
#3356=ORIENTED_EDGE('',*,*,#2423,.T.);
#3357=ORIENTED_EDGE('',*,*,#2394,.T.);
#3358=ORIENTED_EDGE('',*,*,#2383,.T.);
#3359=ORIENTED_EDGE('',*,*,#2487,.T.);
#3360=ORIENTED_EDGE('',*,*,#2387,.T.);
#3361=ORIENTED_EDGE('',*,*,#2489,.T.);
#3362=ORIENTED_EDGE('',*,*,#2385,.F.);
#3363=ORIENTED_EDGE('',*,*,#2488,.F.);
#3364=ORIENTED_EDGE('',*,*,#2393,.F.);
#3365=ORIENTED_EDGE('',*,*,#2486,.F.);
#3366=ORIENTED_EDGE('',*,*,#2490,.T.);
#3367=ORIENTED_EDGE('',*,*,#2491,.T.);
#3368=ORIENTED_EDGE('',*,*,#2492,.F.);
#3369=ORIENTED_EDGE('',*,*,#2491,.F.);
#3370=ORIENTED_EDGE('',*,*,#2493,.T.);
#3371=ORIENTED_EDGE('',*,*,#2494,.T.);
#3372=ORIENTED_EDGE('',*,*,#2495,.F.);
#3373=ORIENTED_EDGE('',*,*,#2494,.F.);
#3374=ORIENTED_EDGE('',*,*,#2496,.F.);
#3375=ORIENTED_EDGE('',*,*,#2497,.T.);
#3376=ORIENTED_EDGE('',*,*,#2498,.T.);
#3377=ORIENTED_EDGE('',*,*,#2499,.F.);
#3378=ORIENTED_EDGE('',*,*,#2496,.T.);
#3379=ORIENTED_EDGE('',*,*,#2500,.T.);
#3380=ORIENTED_EDGE('',*,*,#2501,.T.);
#3381=ORIENTED_EDGE('',*,*,#2502,.T.);
#3382=ORIENTED_EDGE('',*,*,#2490,.F.);
#3383=ORIENTED_EDGE('',*,*,#2493,.F.);
#3384=ORIENTED_EDGE('',*,*,#2498,.F.);
#3385=ORIENTED_EDGE('',*,*,#2503,.F.);
#3386=ORIENTED_EDGE('',*,*,#2504,.F.);
#3387=ORIENTED_EDGE('',*,*,#2505,.F.);
#3388=ORIENTED_EDGE('',*,*,#2492,.T.);
#3389=ORIENTED_EDGE('',*,*,#2495,.T.);
#3390=ORIENTED_EDGE('',*,*,#2505,.T.);
#3391=ORIENTED_EDGE('',*,*,#2506,.F.);
#3392=ORIENTED_EDGE('',*,*,#2500,.F.);
#3393=ORIENTED_EDGE('',*,*,#2499,.T.);
#3394=ORIENTED_EDGE('',*,*,#2504,.T.);
#3395=ORIENTED_EDGE('',*,*,#2507,.F.);
#3396=ORIENTED_EDGE('',*,*,#2501,.F.);
#3397=ORIENTED_EDGE('',*,*,#2506,.T.);
#3398=ORIENTED_EDGE('',*,*,#2503,.T.);
#3399=ORIENTED_EDGE('',*,*,#2497,.F.);
#3400=ORIENTED_EDGE('',*,*,#2502,.F.);
#3401=ORIENTED_EDGE('',*,*,#2507,.T.);
#3402=ORIENTED_EDGE('',*,*,#2508,.F.);
#3403=ORIENTED_EDGE('',*,*,#2509,.T.);
#3404=ORIENTED_EDGE('',*,*,#2510,.F.);
#3405=ORIENTED_EDGE('',*,*,#2509,.F.);
#3406=ORIENTED_EDGE('',*,*,#2511,.F.);
#3407=ORIENTED_EDGE('',*,*,#2512,.T.);
#3408=ORIENTED_EDGE('',*,*,#2513,.F.);
#3409=ORIENTED_EDGE('',*,*,#2512,.F.);
#3410=ORIENTED_EDGE('',*,*,#2514,.F.);
#3411=ORIENTED_EDGE('',*,*,#2515,.F.);
#3412=ORIENTED_EDGE('',*,*,#2516,.T.);
#3413=ORIENTED_EDGE('',*,*,#2517,.F.);
#3414=ORIENTED_EDGE('',*,*,#2516,.F.);
#3415=ORIENTED_EDGE('',*,*,#2518,.F.);
#3416=ORIENTED_EDGE('',*,*,#2519,.F.);
#3417=ORIENTED_EDGE('',*,*,#2520,.T.);
#3418=ORIENTED_EDGE('',*,*,#2521,.F.);
#3419=ORIENTED_EDGE('',*,*,#2520,.F.);
#3420=ORIENTED_EDGE('',*,*,#2522,.T.);
#3421=ORIENTED_EDGE('',*,*,#2523,.T.);
#3422=ORIENTED_EDGE('',*,*,#2511,.T.);
#3423=ORIENTED_EDGE('',*,*,#2523,.F.);
#3424=ORIENTED_EDGE('',*,*,#2518,.T.);
#3425=ORIENTED_EDGE('',*,*,#2519,.T.);
#3426=ORIENTED_EDGE('',*,*,#2524,.T.);
#3427=ORIENTED_EDGE('',*,*,#2525,.F.);
#3428=ORIENTED_EDGE('',*,*,#2524,.F.);
#3429=ORIENTED_EDGE('',*,*,#2526,.T.);
#3430=ORIENTED_EDGE('',*,*,#2527,.T.);
#3431=ORIENTED_EDGE('',*,*,#2528,.T.);
#3432=ORIENTED_EDGE('',*,*,#2527,.F.);
#3433=ORIENTED_EDGE('',*,*,#2529,.T.);
#3434=ORIENTED_EDGE('',*,*,#2530,.T.);
#3435=ORIENTED_EDGE('',*,*,#2508,.T.);
#3436=ORIENTED_EDGE('',*,*,#2530,.F.);
#3437=ORIENTED_EDGE('',*,*,#2514,.T.);
#3438=ORIENTED_EDGE('',*,*,#2515,.T.);
#3439=ORIENTED_EDGE('',*,*,#2531,.T.);
#3440=ORIENTED_EDGE('',*,*,#2532,.F.);
#3441=ORIENTED_EDGE('',*,*,#2531,.F.);
#3442=ORIENTED_EDGE('',*,*,#2533,.F.);
#3443=ORIENTED_EDGE('',*,*,#2534,.F.);
#3444=ORIENTED_EDGE('',*,*,#2535,.F.);
#3445=ORIENTED_EDGE('',*,*,#2536,.T.);
#3446=ORIENTED_EDGE('',*,*,#2537,.F.);
#3447=ORIENTED_EDGE('',*,*,#2538,.F.);
#3448=ORIENTED_EDGE('',*,*,#2539,.F.);
#3449=ORIENTED_EDGE('',*,*,#2540,.T.);
#3450=ORIENTED_EDGE('',*,*,#2541,.F.);
#3451=ORIENTED_EDGE('',*,*,#2542,.F.);
#3452=ORIENTED_EDGE('',*,*,#2543,.F.);
#3453=ORIENTED_EDGE('',*,*,#2544,.F.);
#3454=ORIENTED_EDGE('',*,*,#2545,.F.);
#3455=ORIENTED_EDGE('',*,*,#2546,.F.);
#3456=ORIENTED_EDGE('',*,*,#2547,.T.);
#3457=ORIENTED_EDGE('',*,*,#2548,.T.);
#3458=ORIENTED_EDGE('',*,*,#2547,.F.);
#3459=ORIENTED_EDGE('',*,*,#2533,.T.);
#3460=ORIENTED_EDGE('',*,*,#2549,.T.);
#3461=ORIENTED_EDGE('',*,*,#2550,.F.);
#3462=ORIENTED_EDGE('',*,*,#2551,.F.);
#3463=ORIENTED_EDGE('',*,*,#2552,.T.);
#3464=ORIENTED_EDGE('',*,*,#2553,.T.);
#3465=ORIENTED_EDGE('',*,*,#2554,.F.);
#3466=ORIENTED_EDGE('',*,*,#2553,.F.);
#3467=ORIENTED_EDGE('',*,*,#2555,.T.);
#3468=ORIENTED_EDGE('',*,*,#2556,.T.);
#3469=ORIENTED_EDGE('',*,*,#2557,.T.);
#3470=ORIENTED_EDGE('',*,*,#2558,.F.);
#3471=ORIENTED_EDGE('',*,*,#2559,.T.);
#3472=ORIENTED_EDGE('',*,*,#2560,.T.);
#3473=ORIENTED_EDGE('',*,*,#2561,.T.);
#3474=ORIENTED_EDGE('',*,*,#2562,.T.);
#3475=ORIENTED_EDGE('',*,*,#2563,.T.);
#3476=ORIENTED_EDGE('',*,*,#2564,.F.);
#3477=ORIENTED_EDGE('',*,*,#2565,.T.);
#3478=ORIENTED_EDGE('',*,*,#2566,.T.);
#3479=ORIENTED_EDGE('',*,*,#2537,.T.);
#3480=ORIENTED_EDGE('',*,*,#2567,.T.);
#3481=ORIENTED_EDGE('',*,*,#2568,.F.);
#3482=ORIENTED_EDGE('',*,*,#2567,.F.);
#3483=ORIENTED_EDGE('',*,*,#2541,.T.);
#3484=ORIENTED_EDGE('',*,*,#2569,.T.);
#3485=ORIENTED_EDGE('',*,*,#2570,.T.);
#3486=ORIENTED_EDGE('',*,*,#2571,.T.);
#3487=ORIENTED_EDGE('',*,*,#2572,.T.);
#3488=ORIENTED_EDGE('',*,*,#2560,.F.);
#3489=ORIENTED_EDGE('',*,*,#2573,.T.);
#3490=ORIENTED_EDGE('',*,*,#2574,.T.);
#3491=ORIENTED_EDGE('',*,*,#2575,.T.);
#3492=ORIENTED_EDGE('',*,*,#2576,.T.);
#3493=ORIENTED_EDGE('',*,*,#2577,.T.);
#3494=ORIENTED_EDGE('',*,*,#2578,.T.);
#3495=ORIENTED_EDGE('',*,*,#2579,.T.);
#3496=ORIENTED_EDGE('',*,*,#2539,.T.);
#3497=ORIENTED_EDGE('',*,*,#2522,.F.);
#3498=ORIENTED_EDGE('',*,*,#2556,.F.);
#3499=ORIENTED_EDGE('',*,*,#2580,.T.);
#3500=ORIENTED_EDGE('',*,*,#2564,.T.);
#3501=ORIENTED_EDGE('',*,*,#2581,.T.);
#3502=ORIENTED_EDGE('',*,*,#2551,.T.);
#3503=ORIENTED_EDGE('',*,*,#2582,.F.);
#3504=ORIENTED_EDGE('',*,*,#2583,.F.);
#3505=ORIENTED_EDGE('',*,*,#2584,.T.);
#3506=ORIENTED_EDGE('',*,*,#2585,.F.);
#3507=ORIENTED_EDGE('',*,*,#2586,.T.);
#3508=ORIENTED_EDGE('',*,*,#2558,.T.);
#3509=ORIENTED_EDGE('',*,*,#2587,.T.);
#3510=ORIENTED_EDGE('',*,*,#2588,.T.);
#3511=ORIENTED_EDGE('',*,*,#2589,.F.);
#3512=ORIENTED_EDGE('',*,*,#2549,.F.);
#3513=ORIENTED_EDGE('',*,*,#2590,.T.);
#3514=ORIENTED_EDGE('',*,*,#2591,.F.);
#3515=ORIENTED_EDGE('',*,*,#2592,.T.);
#3516=ORIENTED_EDGE('',*,*,#2585,.T.);
#3517=ORIENTED_EDGE('',*,*,#2593,.T.);
#3518=ORIENTED_EDGE('',*,*,#2594,.F.);
#3519=ORIENTED_EDGE('',*,*,#2595,.T.);
#3520=ORIENTED_EDGE('',*,*,#2596,.T.);
#3521=ORIENTED_EDGE('',*,*,#2597,.T.);
#3522=ORIENTED_EDGE('',*,*,#2598,.F.);
#3523=ORIENTED_EDGE('',*,*,#2599,.T.);
#3524=ORIENTED_EDGE('',*,*,#2591,.T.);
#3525=ORIENTED_EDGE('',*,*,#2600,.T.);
#3526=ORIENTED_EDGE('',*,*,#2601,.F.);
#3527=ORIENTED_EDGE('',*,*,#2602,.T.);
#3528=ORIENTED_EDGE('',*,*,#2603,.T.);
#3529=ORIENTED_EDGE('',*,*,#2604,.T.);
#3530=ORIENTED_EDGE('',*,*,#2605,.T.);
#3531=ORIENTED_EDGE('',*,*,#2606,.F.);
#3532=ORIENTED_EDGE('',*,*,#2607,.F.);
#3533=ORIENTED_EDGE('',*,*,#2608,.T.);
#3534=ORIENTED_EDGE('',*,*,#2609,.T.);
#3535=ORIENTED_EDGE('',*,*,#2610,.T.);
#3536=ORIENTED_EDGE('',*,*,#2611,.T.);
#3537=ORIENTED_EDGE('',*,*,#2612,.T.);
#3538=ORIENTED_EDGE('',*,*,#2613,.T.);
#3539=ORIENTED_EDGE('',*,*,#2614,.F.);
#3540=ORIENTED_EDGE('',*,*,#2615,.F.);
#3541=ORIENTED_EDGE('',*,*,#2616,.T.);
#3542=ORIENTED_EDGE('',*,*,#2617,.T.);
#3543=ORIENTED_EDGE('',*,*,#2618,.T.);
#3544=ORIENTED_EDGE('',*,*,#2619,.F.);
#3545=ORIENTED_EDGE('',*,*,#2620,.T.);
#3546=ORIENTED_EDGE('',*,*,#2570,.F.);
#3547=ORIENTED_EDGE('',*,*,#2621,.T.);
#3548=ORIENTED_EDGE('',*,*,#2622,.F.);
#3549=ORIENTED_EDGE('',*,*,#2623,.T.);
#3550=ORIENTED_EDGE('',*,*,#2624,.T.);
#3551=ORIENTED_EDGE('',*,*,#2625,.T.);
#3552=ORIENTED_EDGE('',*,*,#2544,.T.);
#3553=ORIENTED_EDGE('',*,*,#2626,.T.);
#3554=ORIENTED_EDGE('',*,*,#2552,.F.);
#3555=ORIENTED_EDGE('',*,*,#2611,.F.);
#3556=ORIENTED_EDGE('',*,*,#2542,.T.);
#3557=ORIENTED_EDGE('',*,*,#2594,.T.);
#3558=ORIENTED_EDGE('',*,*,#2627,.T.);
#3559=ORIENTED_EDGE('',*,*,#2607,.T.);
#3560=ORIENTED_EDGE('',*,*,#2628,.F.);
#3561=ORIENTED_EDGE('',*,*,#2613,.F.);
#3562=ORIENTED_EDGE('',*,*,#2629,.T.);
#3563=ORIENTED_EDGE('',*,*,#2627,.F.);
#3564=ORIENTED_EDGE('',*,*,#2608,.F.);
#3565=ORIENTED_EDGE('',*,*,#2629,.F.);
#3566=ORIENTED_EDGE('',*,*,#2612,.F.);
#3567=ORIENTED_EDGE('',*,*,#2554,.T.);
#3568=ORIENTED_EDGE('',*,*,#2583,.T.);
#3569=ORIENTED_EDGE('',*,*,#2630,.F.);
#3570=ORIENTED_EDGE('',*,*,#2588,.F.);
#3571=ORIENTED_EDGE('',*,*,#2631,.T.);
#3572=ORIENTED_EDGE('',*,*,#2557,.F.);
#3573=ORIENTED_EDGE('',*,*,#2584,.F.);
#3574=ORIENTED_EDGE('',*,*,#2631,.F.);
#3575=ORIENTED_EDGE('',*,*,#2587,.F.);
#3576=ORIENTED_EDGE('',*,*,#2528,.F.);
#3577=ORIENTED_EDGE('',*,*,#2632,.T.);
#3578=ORIENTED_EDGE('',*,*,#2633,.T.);
#3579=ORIENTED_EDGE('',*,*,#2634,.T.);
#3580=ORIENTED_EDGE('',*,*,#2635,.T.);
#3581=ORIENTED_EDGE('',*,*,#2568,.T.);
#3582=ORIENTED_EDGE('',*,*,#2529,.F.);
#3583=ORIENTED_EDGE('',*,*,#2636,.T.);
#3584=ORIENTED_EDGE('',*,*,#2535,.T.);
#3585=ORIENTED_EDGE('',*,*,#2637,.T.);
#3586=ORIENTED_EDGE('',*,*,#2638,.T.);
#3587=ORIENTED_EDGE('',*,*,#2639,.T.);
#3588=ORIENTED_EDGE('',*,*,#2640,.T.);
#3589=ORIENTED_EDGE('',*,*,#2641,.T.);
#3590=ORIENTED_EDGE('',*,*,#2642,.T.);
#3591=ORIENTED_EDGE('',*,*,#2525,.T.);
#3592=ORIENTED_EDGE('',*,*,#2643,.T.);
#3593=ORIENTED_EDGE('',*,*,#2644,.T.);
#3594=ORIENTED_EDGE('',*,*,#2645,.T.);
#3595=ORIENTED_EDGE('',*,*,#2646,.T.);
#3596=ORIENTED_EDGE('',*,*,#2546,.T.);
#3597=ORIENTED_EDGE('',*,*,#2605,.F.);
#3598=ORIENTED_EDGE('',*,*,#2647,.T.);
#3599=ORIENTED_EDGE('',*,*,#2615,.T.);
#3600=ORIENTED_EDGE('',*,*,#2648,.F.);
#3601=ORIENTED_EDGE('',*,*,#2648,.T.);
#3602=ORIENTED_EDGE('',*,*,#2614,.T.);
#3603=ORIENTED_EDGE('',*,*,#2628,.T.);
#3604=ORIENTED_EDGE('',*,*,#2606,.T.);
#3605=ORIENTED_EDGE('',*,*,#2548,.F.);
#3606=ORIENTED_EDGE('',*,*,#2550,.T.);
#3607=ORIENTED_EDGE('',*,*,#2589,.T.);
#3608=ORIENTED_EDGE('',*,*,#2630,.T.);
#3609=ORIENTED_EDGE('',*,*,#2582,.T.);
#3610=ORIENTED_EDGE('',*,*,#2526,.F.);
#3611=ORIENTED_EDGE('',*,*,#2649,.T.);
#3612=ORIENTED_EDGE('',*,*,#2650,.T.);
#3613=ORIENTED_EDGE('',*,*,#2651,.T.);
#3614=ORIENTED_EDGE('',*,*,#2652,.T.);
#3615=ORIENTED_EDGE('',*,*,#2559,.F.);
#3616=ORIENTED_EDGE('',*,*,#2532,.T.);
#3617=ORIENTED_EDGE('',*,*,#2645,.F.);
#3618=ORIENTED_EDGE('',*,*,#2653,.T.);
#3619=ORIENTED_EDGE('',*,*,#2649,.F.);
#3620=ORIENTED_EDGE('',*,*,#2654,.T.);
#3621=ORIENTED_EDGE('',*,*,#2624,.F.);
#3622=ORIENTED_EDGE('',*,*,#2655,.T.);
#3623=ORIENTED_EDGE('',*,*,#2632,.F.);
#3624=ORIENTED_EDGE('',*,*,#2656,.T.);
#3625=ORIENTED_EDGE('',*,*,#2543,.T.);
#3626=ORIENTED_EDGE('',*,*,#2610,.F.);
#3627=ORIENTED_EDGE('',*,*,#2657,.F.);
#3628=ORIENTED_EDGE('',*,*,#2626,.F.);
#3629=ORIENTED_EDGE('',*,*,#2545,.T.);
#3630=ORIENTED_EDGE('',*,*,#2625,.F.);
#3631=ORIENTED_EDGE('',*,*,#2658,.F.);
#3632=ORIENTED_EDGE('',*,*,#2595,.F.);
#3633=ORIENTED_EDGE('',*,*,#2657,.T.);
#3634=ORIENTED_EDGE('',*,*,#2609,.F.);
#3635=ORIENTED_EDGE('',*,*,#2659,.F.);
#3636=ORIENTED_EDGE('',*,*,#2655,.F.);
#3637=ORIENTED_EDGE('',*,*,#2658,.T.);
#3638=ORIENTED_EDGE('',*,*,#2656,.F.);
#3639=ORIENTED_EDGE('',*,*,#2660,.F.);
#3640=ORIENTED_EDGE('',*,*,#2596,.F.);
#3641=ORIENTED_EDGE('',*,*,#2659,.T.);
#3642=ORIENTED_EDGE('',*,*,#2623,.F.);
#3643=ORIENTED_EDGE('',*,*,#2661,.F.);
#3644=ORIENTED_EDGE('',*,*,#2633,.F.);
#3645=ORIENTED_EDGE('',*,*,#2662,.F.);
#3646=ORIENTED_EDGE('',*,*,#2634,.F.);
#3647=ORIENTED_EDGE('',*,*,#2663,.F.);
#3648=ORIENTED_EDGE('',*,*,#2578,.F.);
#3649=ORIENTED_EDGE('',*,*,#2660,.T.);
#3650=ORIENTED_EDGE('',*,*,#2635,.F.);
#3651=ORIENTED_EDGE('',*,*,#2664,.F.);
#3652=ORIENTED_EDGE('',*,*,#2597,.F.);
#3653=ORIENTED_EDGE('',*,*,#2661,.T.);
#3654=ORIENTED_EDGE('',*,*,#2622,.T.);
#3655=ORIENTED_EDGE('',*,*,#2665,.F.);
#3656=ORIENTED_EDGE('',*,*,#2663,.T.);
#3657=ORIENTED_EDGE('',*,*,#2664,.T.);
#3658=ORIENTED_EDGE('',*,*,#2662,.T.);
#3659=ORIENTED_EDGE('',*,*,#2666,.F.);
#3660=ORIENTED_EDGE('',*,*,#2598,.T.);
#3661=ORIENTED_EDGE('',*,*,#2665,.T.);
#3662=ORIENTED_EDGE('',*,*,#2621,.F.);
#3663=ORIENTED_EDGE('',*,*,#2667,.F.);
#3664=ORIENTED_EDGE('',*,*,#2579,.F.);
#3665=ORIENTED_EDGE('',*,*,#2666,.T.);
#3666=ORIENTED_EDGE('',*,*,#2577,.F.);
#3667=ORIENTED_EDGE('',*,*,#2668,.F.);
#3668=ORIENTED_EDGE('',*,*,#2599,.F.);
#3669=ORIENTED_EDGE('',*,*,#2667,.T.);
#3670=ORIENTED_EDGE('',*,*,#2569,.F.);
#3671=ORIENTED_EDGE('',*,*,#2540,.F.);
#3672=ORIENTED_EDGE('',*,*,#2668,.T.);
#3673=ORIENTED_EDGE('',*,*,#2576,.F.);
#3674=ORIENTED_EDGE('',*,*,#2669,.F.);
#3675=ORIENTED_EDGE('',*,*,#2592,.F.);
#3676=ORIENTED_EDGE('',*,*,#2669,.T.);
#3677=ORIENTED_EDGE('',*,*,#2575,.F.);
#3678=ORIENTED_EDGE('',*,*,#2670,.F.);
#3679=ORIENTED_EDGE('',*,*,#2586,.F.);
#3680=ORIENTED_EDGE('',*,*,#2538,.T.);
#3681=ORIENTED_EDGE('',*,*,#2566,.F.);
#3682=ORIENTED_EDGE('',*,*,#2565,.F.);
#3683=ORIENTED_EDGE('',*,*,#2671,.F.);
#3684=ORIENTED_EDGE('',*,*,#2670,.T.);
#3685=ORIENTED_EDGE('',*,*,#2574,.F.);
#3686=ORIENTED_EDGE('',*,*,#2672,.F.);
#3687=ORIENTED_EDGE('',*,*,#2555,.F.);
#3688=ORIENTED_EDGE('',*,*,#2671,.T.);
#3689=ORIENTED_EDGE('',*,*,#2580,.F.);
#3690=ORIENTED_EDGE('',*,*,#2672,.T.);
#3691=ORIENTED_EDGE('',*,*,#2573,.F.);
#3692=ORIENTED_EDGE('',*,*,#2673,.F.);
#3693=ORIENTED_EDGE('',*,*,#2643,.F.);
#3694=ORIENTED_EDGE('',*,*,#2674,.F.);
#3695=ORIENTED_EDGE('',*,*,#2647,.F.);
#3696=ORIENTED_EDGE('',*,*,#2674,.T.);
#3697=ORIENTED_EDGE('',*,*,#2646,.F.);
#3698=ORIENTED_EDGE('',*,*,#2675,.F.);
#3699=ORIENTED_EDGE('',*,*,#2616,.F.);
#3700=ORIENTED_EDGE('',*,*,#2673,.T.);
#3701=ORIENTED_EDGE('',*,*,#2604,.F.);
#3702=ORIENTED_EDGE('',*,*,#2676,.F.);
#3703=ORIENTED_EDGE('',*,*,#2644,.F.);
#3704=ORIENTED_EDGE('',*,*,#2675,.T.);
#3705=ORIENTED_EDGE('',*,*,#2654,.F.);
#3706=ORIENTED_EDGE('',*,*,#2677,.F.);
#3707=ORIENTED_EDGE('',*,*,#2617,.F.);
#3708=ORIENTED_EDGE('',*,*,#2676,.T.);
#3709=ORIENTED_EDGE('',*,*,#2603,.F.);
#3710=ORIENTED_EDGE('',*,*,#2678,.F.);
#3711=ORIENTED_EDGE('',*,*,#2653,.F.);
#3712=ORIENTED_EDGE('',*,*,#2677,.T.);
#3713=ORIENTED_EDGE('',*,*,#2652,.F.);
#3714=ORIENTED_EDGE('',*,*,#2679,.F.);
#3715=ORIENTED_EDGE('',*,*,#2618,.F.);
#3716=ORIENTED_EDGE('',*,*,#2678,.T.);
#3717=ORIENTED_EDGE('',*,*,#2602,.F.);
#3718=ORIENTED_EDGE('',*,*,#2680,.F.);
#3719=ORIENTED_EDGE('',*,*,#2650,.F.);
#3720=ORIENTED_EDGE('',*,*,#2681,.F.);
#3721=ORIENTED_EDGE('',*,*,#2651,.F.);
#3722=ORIENTED_EDGE('',*,*,#2682,.F.);
#3723=ORIENTED_EDGE('',*,*,#2640,.F.);
#3724=ORIENTED_EDGE('',*,*,#2679,.T.);
#3725=ORIENTED_EDGE('',*,*,#2681,.T.);
#3726=ORIENTED_EDGE('',*,*,#2683,.F.);
#3727=ORIENTED_EDGE('',*,*,#2619,.T.);
#3728=ORIENTED_EDGE('',*,*,#2680,.T.);
#3729=ORIENTED_EDGE('',*,*,#2601,.T.);
#3730=ORIENTED_EDGE('',*,*,#2684,.F.);
#3731=ORIENTED_EDGE('',*,*,#2682,.T.);
#3732=ORIENTED_EDGE('',*,*,#2683,.T.);
#3733=ORIENTED_EDGE('',*,*,#2639,.F.);
#3734=ORIENTED_EDGE('',*,*,#2685,.F.);
#3735=ORIENTED_EDGE('',*,*,#2620,.F.);
#3736=ORIENTED_EDGE('',*,*,#2684,.T.);
#3737=ORIENTED_EDGE('',*,*,#2600,.F.);
#3738=ORIENTED_EDGE('',*,*,#2686,.F.);
#3739=ORIENTED_EDGE('',*,*,#2641,.F.);
#3740=ORIENTED_EDGE('',*,*,#2571,.F.);
#3741=ORIENTED_EDGE('',*,*,#2685,.T.);
#3742=ORIENTED_EDGE('',*,*,#2687,.F.);
#3743=ORIENTED_EDGE('',*,*,#2686,.T.);
#3744=ORIENTED_EDGE('',*,*,#2593,.F.);
#3745=ORIENTED_EDGE('',*,*,#2688,.F.);
#3746=ORIENTED_EDGE('',*,*,#2642,.F.);
#3747=ORIENTED_EDGE('',*,*,#2687,.T.);
#3748=ORIENTED_EDGE('',*,*,#2638,.F.);
#3749=ORIENTED_EDGE('',*,*,#2689,.F.);
#3750=ORIENTED_EDGE('',*,*,#2561,.F.);
#3751=ORIENTED_EDGE('',*,*,#2572,.F.);
#3752=ORIENTED_EDGE('',*,*,#2688,.T.);
#3753=ORIENTED_EDGE('',*,*,#2590,.F.);
#3754=ORIENTED_EDGE('',*,*,#2536,.F.);
#3755=ORIENTED_EDGE('',*,*,#2636,.F.);
#3756=ORIENTED_EDGE('',*,*,#2562,.F.);
#3757=ORIENTED_EDGE('',*,*,#2689,.T.);
#3758=ORIENTED_EDGE('',*,*,#2690,.F.);
#3759=ORIENTED_EDGE('',*,*,#2563,.F.);
#3760=ORIENTED_EDGE('',*,*,#2690,.T.);
#3761=ORIENTED_EDGE('',*,*,#2637,.F.);
#3762=ORIENTED_EDGE('',*,*,#2534,.T.);
#3763=ORIENTED_EDGE('',*,*,#2581,.F.);
#3764=ORIENTED_EDGE('',*,*,#2517,.T.);
#3765=ORIENTED_EDGE('',*,*,#2510,.T.);
#3766=ORIENTED_EDGE('',*,*,#2521,.T.);
#3767=ORIENTED_EDGE('',*,*,#2513,.T.);
#3768=ORIENTED_EDGE('',*,*,#2691,.T.);
#3769=ORIENTED_EDGE('',*,*,#2692,.T.);
#3770=ORIENTED_EDGE('',*,*,#2693,.F.);
#3771=ORIENTED_EDGE('',*,*,#2692,.F.);
#3772=ORIENTED_EDGE('',*,*,#2694,.T.);
#3773=ORIENTED_EDGE('',*,*,#2695,.T.);
#3774=ORIENTED_EDGE('',*,*,#2696,.F.);
#3775=ORIENTED_EDGE('',*,*,#2695,.F.);
#3776=ORIENTED_EDGE('',*,*,#2697,.F.);
#3777=ORIENTED_EDGE('',*,*,#2698,.T.);
#3778=ORIENTED_EDGE('',*,*,#2699,.T.);
#3779=ORIENTED_EDGE('',*,*,#2700,.F.);
#3780=ORIENTED_EDGE('',*,*,#2697,.T.);
#3781=ORIENTED_EDGE('',*,*,#2701,.T.);
#3782=ORIENTED_EDGE('',*,*,#2702,.T.);
#3783=ORIENTED_EDGE('',*,*,#2703,.T.);
#3784=ORIENTED_EDGE('',*,*,#2691,.F.);
#3785=ORIENTED_EDGE('',*,*,#2694,.F.);
#3786=ORIENTED_EDGE('',*,*,#2699,.F.);
#3787=ORIENTED_EDGE('',*,*,#2704,.F.);
#3788=ORIENTED_EDGE('',*,*,#2705,.F.);
#3789=ORIENTED_EDGE('',*,*,#2706,.F.);
#3790=ORIENTED_EDGE('',*,*,#2693,.T.);
#3791=ORIENTED_EDGE('',*,*,#2696,.T.);
#3792=ORIENTED_EDGE('',*,*,#2706,.T.);
#3793=ORIENTED_EDGE('',*,*,#2707,.F.);
#3794=ORIENTED_EDGE('',*,*,#2701,.F.);
#3795=ORIENTED_EDGE('',*,*,#2700,.T.);
#3796=ORIENTED_EDGE('',*,*,#2705,.T.);
#3797=ORIENTED_EDGE('',*,*,#2708,.F.);
#3798=ORIENTED_EDGE('',*,*,#2702,.F.);
#3799=ORIENTED_EDGE('',*,*,#2707,.T.);
#3800=ORIENTED_EDGE('',*,*,#2704,.T.);
#3801=ORIENTED_EDGE('',*,*,#2698,.F.);
#3802=ORIENTED_EDGE('',*,*,#2703,.F.);
#3803=ORIENTED_EDGE('',*,*,#2708,.T.);
#3804=ORIENTED_EDGE('',*,*,#2709,.F.);
#3805=ORIENTED_EDGE('',*,*,#2710,.F.);
#3806=ORIENTED_EDGE('',*,*,#2711,.T.);
#3807=ORIENTED_EDGE('',*,*,#2712,.F.);
#3808=ORIENTED_EDGE('',*,*,#2711,.F.);
#3809=ORIENTED_EDGE('',*,*,#2713,.F.);
#3810=ORIENTED_EDGE('',*,*,#2714,.F.);
#3811=ORIENTED_EDGE('',*,*,#2715,.T.);
#3812=ORIENTED_EDGE('',*,*,#2716,.F.);
#3813=ORIENTED_EDGE('',*,*,#2715,.F.);
#3814=ORIENTED_EDGE('',*,*,#2717,.F.);
#3815=ORIENTED_EDGE('',*,*,#2718,.T.);
#3816=ORIENTED_EDGE('',*,*,#2719,.F.);
#3817=ORIENTED_EDGE('',*,*,#2718,.F.);
#3818=ORIENTED_EDGE('',*,*,#2720,.F.);
#3819=ORIENTED_EDGE('',*,*,#2721,.T.);
#3820=ORIENTED_EDGE('',*,*,#2722,.F.);
#3821=ORIENTED_EDGE('',*,*,#2721,.F.);
#3822=ORIENTED_EDGE('',*,*,#2723,.T.);
#3823=ORIENTED_EDGE('',*,*,#2724,.T.);
#3824=ORIENTED_EDGE('',*,*,#2720,.T.);
#3825=ORIENTED_EDGE('',*,*,#2724,.F.);
#3826=ORIENTED_EDGE('',*,*,#2713,.T.);
#3827=ORIENTED_EDGE('',*,*,#2714,.T.);
#3828=ORIENTED_EDGE('',*,*,#2725,.T.);
#3829=ORIENTED_EDGE('',*,*,#2726,.T.);
#3830=ORIENTED_EDGE('',*,*,#2725,.F.);
#3831=ORIENTED_EDGE('',*,*,#2727,.T.);
#3832=ORIENTED_EDGE('',*,*,#2728,.T.);
#3833=ORIENTED_EDGE('',*,*,#2717,.T.);
#3834=ORIENTED_EDGE('',*,*,#2728,.F.);
#3835=ORIENTED_EDGE('',*,*,#2709,.T.);
#3836=ORIENTED_EDGE('',*,*,#2710,.T.);
#3837=ORIENTED_EDGE('',*,*,#2729,.T.);
#3838=ORIENTED_EDGE('',*,*,#2730,.T.);
#3839=ORIENTED_EDGE('',*,*,#2729,.F.);
#3840=ORIENTED_EDGE('',*,*,#2731,.T.);
#3841=ORIENTED_EDGE('',*,*,#2732,.T.);
#3842=ORIENTED_EDGE('',*,*,#2733,.T.);
#3843=ORIENTED_EDGE('',*,*,#2734,.T.);
#3844=ORIENTED_EDGE('',*,*,#2735,.T.);
#3845=ORIENTED_EDGE('',*,*,#2736,.T.);
#3846=ORIENTED_EDGE('',*,*,#2737,.T.);
#3847=ORIENTED_EDGE('',*,*,#2738,.T.);
#3848=ORIENTED_EDGE('',*,*,#2739,.T.);
#3849=ORIENTED_EDGE('',*,*,#2727,.F.);
#3850=ORIENTED_EDGE('',*,*,#2723,.F.);
#3851=ORIENTED_EDGE('',*,*,#2740,.F.);
#3852=ORIENTED_EDGE('',*,*,#2741,.F.);
#3853=ORIENTED_EDGE('',*,*,#2742,.F.);
#3854=ORIENTED_EDGE('',*,*,#2743,.F.);
#3855=ORIENTED_EDGE('',*,*,#2744,.F.);
#3856=ORIENTED_EDGE('',*,*,#2745,.F.);
#3857=ORIENTED_EDGE('',*,*,#2746,.F.);
#3858=ORIENTED_EDGE('',*,*,#2747,.F.);
#3859=ORIENTED_EDGE('',*,*,#2748,.F.);
#3860=ORIENTED_EDGE('',*,*,#2730,.F.);
#3861=ORIENTED_EDGE('',*,*,#2726,.F.);
#3862=ORIENTED_EDGE('',*,*,#2740,.T.);
#3863=ORIENTED_EDGE('',*,*,#2749,.F.);
#3864=ORIENTED_EDGE('',*,*,#2731,.F.);
#3865=ORIENTED_EDGE('',*,*,#2750,.T.);
#3866=ORIENTED_EDGE('',*,*,#2748,.T.);
#3867=ORIENTED_EDGE('',*,*,#2751,.F.);
#3868=ORIENTED_EDGE('',*,*,#2732,.F.);
#3869=ORIENTED_EDGE('',*,*,#2749,.T.);
#3870=ORIENTED_EDGE('',*,*,#2747,.T.);
#3871=ORIENTED_EDGE('',*,*,#2752,.F.);
#3872=ORIENTED_EDGE('',*,*,#2733,.F.);
#3873=ORIENTED_EDGE('',*,*,#2751,.T.);
#3874=ORIENTED_EDGE('',*,*,#2746,.T.);
#3875=ORIENTED_EDGE('',*,*,#2753,.F.);
#3876=ORIENTED_EDGE('',*,*,#2734,.F.);
#3877=ORIENTED_EDGE('',*,*,#2752,.T.);
#3878=ORIENTED_EDGE('',*,*,#2745,.T.);
#3879=ORIENTED_EDGE('',*,*,#2754,.F.);
#3880=ORIENTED_EDGE('',*,*,#2735,.F.);
#3881=ORIENTED_EDGE('',*,*,#2753,.T.);
#3882=ORIENTED_EDGE('',*,*,#2744,.T.);
#3883=ORIENTED_EDGE('',*,*,#2755,.F.);
#3884=ORIENTED_EDGE('',*,*,#2736,.F.);
#3885=ORIENTED_EDGE('',*,*,#2754,.T.);
#3886=ORIENTED_EDGE('',*,*,#2743,.T.);
#3887=ORIENTED_EDGE('',*,*,#2756,.F.);
#3888=ORIENTED_EDGE('',*,*,#2737,.F.);
#3889=ORIENTED_EDGE('',*,*,#2755,.T.);
#3890=ORIENTED_EDGE('',*,*,#2742,.T.);
#3891=ORIENTED_EDGE('',*,*,#2757,.F.);
#3892=ORIENTED_EDGE('',*,*,#2738,.F.);
#3893=ORIENTED_EDGE('',*,*,#2756,.T.);
#3894=ORIENTED_EDGE('',*,*,#2741,.T.);
#3895=ORIENTED_EDGE('',*,*,#2750,.F.);
#3896=ORIENTED_EDGE('',*,*,#2739,.F.);
#3897=ORIENTED_EDGE('',*,*,#2757,.T.);
#3898=ORIENTED_EDGE('',*,*,#2712,.T.);
#3899=ORIENTED_EDGE('',*,*,#2719,.T.);
#3900=ORIENTED_EDGE('',*,*,#2716,.T.);
#3901=ORIENTED_EDGE('',*,*,#2722,.T.);
#3902=TOROIDAL_SURFACE('',#4252,39.2915026221292,8.);
#3903=TOROIDAL_SURFACE('',#4257,4.00000000000002,1.);
#3904=TOROIDAL_SURFACE('',#4263,4.00000000000002,1.);
#3905=TOROIDAL_SURFACE('',#4504,8.,2.);
#3906=TOROIDAL_SURFACE('',#4509,12.,2.);
#3907=TOROIDAL_SURFACE('',#4515,8.,2.);
#3908=TOROIDAL_SURFACE('',#4585,5.,2.);
#3909=TOROIDAL_SURFACE('',#4587,5.,2.);
#3910=TOROIDAL_SURFACE('',#4596,4.,2.);
#3911=TOROIDAL_SURFACE('',#4598,4.,2.);
#3912=TOROIDAL_SURFACE('',#4603,22.,2.);
#3913=TOROIDAL_SURFACE('',#4607,8.,2.);
#3914=TOROIDAL_SURFACE('',#4610,8.,2.);
#3915=TOROIDAL_SURFACE('',#4617,5.,2.);
#3916=TOROIDAL_SURFACE('',#4619,5.,2.);
#3917=TOROIDAL_SURFACE('',#4628,4.,2.);
#3918=TOROIDAL_SURFACE('',#4630,4.,2.);
#3919=TOROIDAL_SURFACE('',#4636,22.,2.);
#3920=TOROIDAL_SURFACE('',#4638,12.,2.);
#3921=ADVANCED_FACE('',(#1086),#3902,.F.);
#3922=ADVANCED_FACE('',(#1087),#3903,.T.);
#3923=ADVANCED_FACE('',(#1088),#1007,.T.);
#3924=ADVANCED_FACE('',(#1089),#3904,.T.);
#3925=ADVANCED_FACE('',(#1090),#1008,.T.);
#3926=ADVANCED_FACE('',(#1091),#1009,.F.);
#3927=ADVANCED_FACE('',(#1092),#1010,.F.);
#3928=ADVANCED_FACE('',(#1093),#1011,.F.);
#3929=ADVANCED_FACE('',(#1094),#1012,.F.);
#3930=ADVANCED_FACE('',(#1095),#1013,.F.);
#3931=ADVANCED_FACE('',(#1096),#1014,.F.);
#3932=ADVANCED_FACE('',(#1097),#1015,.T.);
#3933=ADVANCED_FACE('',(#1098),#1016,.T.);
#3934=ADVANCED_FACE('',(#1099),#1017,.T.);
#3935=ADVANCED_FACE('',(#1100,#112,#113,#114,#115),#159,.T.);
#3936=ADVANCED_FACE('',(#1101),#160,.F.);
#3937=ADVANCED_FACE('',(#1102),#161,.T.);
#3938=ADVANCED_FACE('',(#1103),#162,.F.);
#3939=ADVANCED_FACE('',(#1104,#116),#163,.F.);
#3940=ADVANCED_FACE('',(#1105),#164,.F.);
#3941=ADVANCED_FACE('',(#1106),#103,.T.);
#3942=ADVANCED_FACE('',(#1107),#165,.F.);
#3943=ADVANCED_FACE('',(#1108),#166,.F.);
#3944=ADVANCED_FACE('',(#1109),#167,.F.);
#3945=ADVANCED_FACE('',(#1110,#117,#118),#168,.F.);
#3946=ADVANCED_FACE('',(#1111),#169,.F.);
#3947=ADVANCED_FACE('',(#1112),#170,.F.);
#3948=ADVANCED_FACE('',(#1113),#1018,.T.);
#3949=ADVANCED_FACE('',(#1114),#171,.F.);
#3950=ADVANCED_FACE('',(#1115),#172,.F.);
#3951=ADVANCED_FACE('',(#1116),#173,.F.);
#3952=ADVANCED_FACE('',(#1117),#1019,.T.);
#3953=ADVANCED_FACE('',(#1118),#174,.F.);
#3954=ADVANCED_FACE('',(#1119),#175,.F.);
#3955=ADVANCED_FACE('',(#1120),#176,.F.);
#3956=ADVANCED_FACE('',(#1121),#177,.F.);
#3957=ADVANCED_FACE('',(#1122),#178,.T.);
#3958=ADVANCED_FACE('',(#1123),#179,.T.);
#3959=ADVANCED_FACE('',(#1124),#180,.F.);
#3960=ADVANCED_FACE('',(#1125),#181,.T.);
#3961=ADVANCED_FACE('',(#1126),#182,.F.);
#3962=ADVANCED_FACE('',(#1127),#183,.F.);
#3963=ADVANCED_FACE('',(#1128),#184,.F.);
#3964=ADVANCED_FACE('',(#1129),#185,.T.);
#3965=ADVANCED_FACE('',(#1130),#186,.F.);
#3966=ADVANCED_FACE('',(#1131),#187,.F.);
#3967=ADVANCED_FACE('',(#1132),#188,.F.);
#3968=ADVANCED_FACE('',(#1133),#189,.F.);
#3969=ADVANCED_FACE('',(#1134),#190,.F.);
#3970=ADVANCED_FACE('',(#1135),#191,.F.);
#3971=ADVANCED_FACE('',(#1136),#192,.F.);
#3972=ADVANCED_FACE('',(#1137),#193,.F.);
#3973=ADVANCED_FACE('',(#1138),#1020,.T.);
#3974=ADVANCED_FACE('',(#1139),#1021,.T.);
#3975=ADVANCED_FACE('',(#1140),#1022,.T.);
#3976=ADVANCED_FACE('',(#1141),#1023,.T.);
#3977=ADVANCED_FACE('',(#1142,#119),#194,.F.);
#3978=ADVANCED_FACE('',(#1143,#120),#195,.F.);
#3979=ADVANCED_FACE('',(#1144),#196,.F.);
#3980=ADVANCED_FACE('',(#1145),#197,.F.);
#3981=ADVANCED_FACE('',(#1146),#198,.F.);
#3982=ADVANCED_FACE('',(#1147),#199,.F.);
#3983=ADVANCED_FACE('',(#1148),#200,.F.);
#3984=ADVANCED_FACE('',(#1149),#201,.F.);
#3985=ADVANCED_FACE('',(#1150),#202,.F.);
#3986=ADVANCED_FACE('',(#1151,#121),#203,.T.);
#3987=ADVANCED_FACE('',(#1152),#204,.F.);
#3988=ADVANCED_FACE('',(#1153),#205,.F.);
#3989=ADVANCED_FACE('',(#1154),#206,.F.);
#3990=ADVANCED_FACE('',(#1155),#207,.F.);
#3991=ADVANCED_FACE('',(#1156),#208,.F.);
#3992=ADVANCED_FACE('',(#1157),#209,.F.);
#3993=ADVANCED_FACE('',(#1158),#210,.F.);
#3994=ADVANCED_FACE('',(#1159),#211,.F.);
#3995=ADVANCED_FACE('',(#1160),#212,.F.);
#3996=ADVANCED_FACE('',(#1161),#213,.F.);
#3997=ADVANCED_FACE('',(#1162),#214,.F.);
#3998=ADVANCED_FACE('',(#1163),#215,.F.);
#3999=ADVANCED_FACE('',(#1164),#216,.F.);
#4000=ADVANCED_FACE('',(#1165,#122),#217,.F.);
#4001=ADVANCED_FACE('',(#1166),#1024,.F.);
#4002=ADVANCED_FACE('',(#1167),#1025,.T.);
#4003=ADVANCED_FACE('',(#1168),#1026,.T.);
#4004=ADVANCED_FACE('',(#1169),#1027,.F.);
#4005=ADVANCED_FACE('',(#1170),#1028,.T.);
#4006=ADVANCED_FACE('',(#1171),#1029,.T.);
#4007=ADVANCED_FACE('',(#1172),#25,.T.);
#4008=ADVANCED_FACE('',(#1173),#1030,.T.);
#4009=ADVANCED_FACE('',(#1174),#1031,.T.);
#4010=ADVANCED_FACE('',(#1175),#1032,.T.);
#4011=ADVANCED_FACE('',(#1176),#26,.T.);
#4012=ADVANCED_FACE('',(#1177),#1033,.T.);
#4013=ADVANCED_FACE('',(#1178),#1034,.T.);
#4014=ADVANCED_FACE('',(#1179),#1035,.T.);
#4015=ADVANCED_FACE('',(#1180),#1036,.F.);
#4016=ADVANCED_FACE('',(#1181,#123),#218,.T.);
#4017=ADVANCED_FACE('',(#1182,#124),#219,.F.);
#4018=ADVANCED_FACE('',(#1183,#125),#220,.F.);
#4019=ADVANCED_FACE('',(#1184,#126),#221,.F.);
#4020=ADVANCED_FACE('',(#1185,#127),#222,.F.);
#4021=ADVANCED_FACE('',(#1186,#128),#223,.F.);
#4022=ADVANCED_FACE('',(#1187,#129),#224,.F.);
#4023=ADVANCED_FACE('',(#1188,#130),#225,.F.);
#4024=ADVANCED_FACE('',(#1189,#131),#226,.F.);
#4025=ADVANCED_FACE('',(#1190,#132),#227,.F.);
#4026=ADVANCED_FACE('',(#1191),#228,.F.);
#4027=ADVANCED_FACE('',(#1192,#133),#229,.F.);
#4028=ADVANCED_FACE('',(#1193),#230,.F.);
#4029=ADVANCED_FACE('',(#1194),#231,.F.);
#4030=ADVANCED_FACE('',(#1195),#232,.F.);
#4031=ADVANCED_FACE('',(#1196,#134),#233,.F.);
#4032=ADVANCED_FACE('',(#1197),#234,.F.);
#4033=ADVANCED_FACE('',(#1198),#235,.F.);
#4034=ADVANCED_FACE('',(#1199),#1037,.T.);
#4035=ADVANCED_FACE('',(#1200),#1038,.T.);
#4036=ADVANCED_FACE('',(#1201),#1039,.T.);
#4037=ADVANCED_FACE('',(#1202),#1040,.T.);
#4038=ADVANCED_FACE('',(#1203),#236,.T.);
#4039=ADVANCED_FACE('',(#1204),#237,.F.);
#4040=ADVANCED_FACE('',(#1205,#135),#238,.T.);
#4041=ADVANCED_FACE('',(#1206,#136),#239,.F.);
#4042=ADVANCED_FACE('',(#1207),#240,.F.);
#4043=ADVANCED_FACE('',(#1208),#241,.F.);
#4044=ADVANCED_FACE('',(#1209),#242,.T.);
#4045=ADVANCED_FACE('',(#1210),#243,.F.);
#4046=ADVANCED_FACE('',(#1211),#1041,.F.);
#4047=ADVANCED_FACE('',(#1212),#1042,.F.);
#4048=ADVANCED_FACE('',(#1213),#1043,.T.);
#4049=ADVANCED_FACE('',(#1214,#137,#138),#244,.T.);
#4050=ADVANCED_FACE('',(#1215,#139,#140),#245,.F.);
#4051=ADVANCED_FACE('',(#1216),#246,.F.);
#4052=ADVANCED_FACE('',(#1217),#1044,.T.);
#4053=ADVANCED_FACE('',(#1218),#247,.F.);
#4054=ADVANCED_FACE('',(#1219),#104,.T.);
#4055=ADVANCED_FACE('',(#1220),#105,.T.);
#4056=ADVANCED_FACE('',(#1221),#106,.T.);
#4057=ADVANCED_FACE('',(#1222),#107,.T.);
#4058=ADVANCED_FACE('',(#1223),#1045,.T.);
#4059=ADVANCED_FACE('',(#1224),#1046,.T.);
#4060=ADVANCED_FACE('',(#1225),#1047,.T.);
#4061=ADVANCED_FACE('',(#1226),#1048,.T.);
#4062=ADVANCED_FACE('',(#1227),#1049,.T.);
#4063=ADVANCED_FACE('',(#1228),#3905,.T.);
#4064=ADVANCED_FACE('',(#1229),#3906,.F.);
#4065=ADVANCED_FACE('',(#1230),#3907,.T.);
#4066=ADVANCED_FACE('',(#1231),#1050,.F.);
#4067=ADVANCED_FACE('',(#1232),#1051,.T.);
#4068=ADVANCED_FACE('',(#1233),#1052,.F.);
#4069=ADVANCED_FACE('',(#1234),#1053,.T.);
#4070=ADVANCED_FACE('',(#1235),#1054,.T.);
#4071=ADVANCED_FACE('',(#1236,#141),#248,.T.);
#4072=ADVANCED_FACE('',(#1237),#249,.F.);
#4073=ADVANCED_FACE('',(#1238),#250,.F.);
#4074=ADVANCED_FACE('',(#1239),#1055,.F.);
#4075=ADVANCED_FACE('',(#1240),#251,.F.);
#4076=ADVANCED_FACE('',(#1241),#252,.F.);
#4077=ADVANCED_FACE('',(#1242,#142),#253,.T.);
#4078=ADVANCED_FACE('',(#1243),#1056,.T.);
#4079=ADVANCED_FACE('',(#1244),#254,.T.);
#4080=ADVANCED_FACE('',(#1245,#143),#255,.F.);
#4081=ADVANCED_FACE('',(#1246),#256,.T.);
#4082=ADVANCED_FACE('',(#1247,#144),#257,.F.);
#4083=ADVANCED_FACE('',(#1248),#258,.F.);
#4084=ADVANCED_FACE('',(#1249,#145),#259,.T.);
#4085=ADVANCED_FACE('',(#1250,#146),#260,.T.);
#4086=ADVANCED_FACE('',(#1251,#147),#261,.T.);
#4087=ADVANCED_FACE('',(#1252),#1057,.T.);
#4088=ADVANCED_FACE('',(#1253,#148),#262,.F.);
#4089=ADVANCED_FACE('',(#1254,#149),#263,.F.);
#4090=ADVANCED_FACE('',(#1255),#264,.F.);
#4091=ADVANCED_FACE('',(#1256,#150),#265,.T.);
#4092=ADVANCED_FACE('',(#1257),#1058,.T.);
#4093=ADVANCED_FACE('',(#1258),#1059,.T.);
#4094=ADVANCED_FACE('',(#1259),#1060,.T.);
#4095=ADVANCED_FACE('',(#1260),#1061,.T.);
#4096=ADVANCED_FACE('',(#1261),#3908,.T.);
#4097=ADVANCED_FACE('',(#1262),#3909,.T.);
#4098=ADVANCED_FACE('',(#1263),#1062,.T.);
#4099=ADVANCED_FACE('',(#1264),#1063,.F.);
#4100=ADVANCED_FACE('',(#1265),#1064,.T.);
#4101=ADVANCED_FACE('',(#1266),#3910,.T.);
#4102=ADVANCED_FACE('',(#1267),#3911,.T.);
#4103=ADVANCED_FACE('',(#1268),#1065,.T.);
#4104=ADVANCED_FACE('',(#1269),#1066,.T.);
#4105=ADVANCED_FACE('',(#1270),#11,.F.);
#4106=ADVANCED_FACE('',(#1271),#3912,.T.);
#4107=ADVANCED_FACE('',(#1272),#1067,.T.);
#4108=ADVANCED_FACE('',(#1273),#12,.F.);
#4109=ADVANCED_FACE('',(#1274),#3913,.T.);
#4110=ADVANCED_FACE('',(#1275),#1068,.T.);
#4111=ADVANCED_FACE('',(#1276),#3914,.T.);
#4112=ADVANCED_FACE('',(#1277),#1069,.T.);
#4113=ADVANCED_FACE('',(#1278),#1070,.T.);
#4114=ADVANCED_FACE('',(#1279),#3915,.T.);
#4115=ADVANCED_FACE('',(#1280),#3916,.T.);
#4116=ADVANCED_FACE('',(#1281),#1071,.T.);
#4117=ADVANCED_FACE('',(#1282),#1072,.T.);
#4118=ADVANCED_FACE('',(#1283),#1073,.F.);
#4119=ADVANCED_FACE('',(#1284),#3917,.T.);
#4120=ADVANCED_FACE('',(#1285),#3918,.T.);
#4121=ADVANCED_FACE('',(#1286),#1074,.T.);
#4122=ADVANCED_FACE('',(#1287),#1075,.T.);
#4123=ADVANCED_FACE('',(#1288),#13,.F.);
#4124=ADVANCED_FACE('',(#1289),#3919,.T.);
#4125=ADVANCED_FACE('',(#1290),#3920,.F.);
#4126=ADVANCED_FACE('',(#1291),#1076,.T.);
#4127=ADVANCED_FACE('',(#1292),#14,.F.);
#4128=ADVANCED_FACE('',(#1293),#1077,.T.);
#4129=ADVANCED_FACE('',(#1294),#266,.F.);
#4130=ADVANCED_FACE('',(#1295),#267,.T.);
#4131=ADVANCED_FACE('',(#1296),#268,.F.);
#4132=ADVANCED_FACE('',(#1297),#269,.T.);
#4133=ADVANCED_FACE('',(#1298),#1078,.F.);
#4134=ADVANCED_FACE('',(#1299),#1079,.F.);
#4135=ADVANCED_FACE('',(#1300),#1080,.T.);
#4136=ADVANCED_FACE('',(#1301,#151,#152),#270,.T.);
#4137=ADVANCED_FACE('',(#1302,#153,#154),#271,.F.);
#4138=ADVANCED_FACE('',(#1303),#272,.F.);
#4139=ADVANCED_FACE('',(#1304),#1081,.T.);
#4140=ADVANCED_FACE('',(#1305),#273,.F.);
#4141=ADVANCED_FACE('',(#1306),#108,.T.);
#4142=ADVANCED_FACE('',(#1307),#109,.T.);
#4143=ADVANCED_FACE('',(#1308),#110,.T.);
#4144=ADVANCED_FACE('',(#1309),#111,.T.);
#4145=ADVANCED_FACE('',(#1310),#1082,.T.);
#4146=ADVANCED_FACE('',(#1311),#1083,.T.);
#4147=ADVANCED_FACE('',(#1312),#1084,.T.);
#4148=ADVANCED_FACE('',(#1313),#1085,.T.);
#4149=ADVANCED_FACE('',(#1314,#155,#156),#274,.T.);
#4150=ADVANCED_FACE('',(#1315,#157,#158),#275,.F.);
#4151=ADVANCED_FACE('',(#1316),#276,.F.);
#4152=ADVANCED_FACE('',(#1317),#277,.F.);
#4153=ADVANCED_FACE('',(#1318),#278,.F.);
#4154=ADVANCED_FACE('',(#1319),#279,.F.);
#4155=ADVANCED_FACE('',(#1320),#280,.F.);
#4156=ADVANCED_FACE('',(#1321),#281,.F.);
#4157=ADVANCED_FACE('',(#1322),#282,.F.);
#4158=ADVANCED_FACE('',(#1323),#283,.F.);
#4159=ADVANCED_FACE('',(#1324),#284,.F.);
#4160=ADVANCED_FACE('',(#1325),#285,.F.);
#4161=ADVANCED_FACE('',(#1326),#286,.T.);
#4162=ADVANCED_FACE('',(#1327),#287,.F.);
#4163=ADVANCED_FACE('',(#1328),#288,.T.);
#4164=CLOSED_SHELL('',(#3921,#3922,#3923,#3924,#3925,#3926,#3927,#3928,
#3929,#3930,#3931,#3932,#3933,#3934,#3935,#3936,#3937,#3938,#3939,#3940,
#3941,#3942,#3943,#3944,#3945,#3946,#3947,#3948,#3949,#3950,#3951,#3952,
#3953,#3954,#3955,#3956,#3957,#3958,#3959,#3960,#3961,#3962,#3963,#3964,
#3965,#3966,#3967,#3968,#3969,#3970,#3971,#3972));
#4165=CLOSED_SHELL('',(#3973,#3974,#3975,#3976,#3977,#3978,#3979,#3980,
#3981,#3982,#3983,#3984,#3985,#3986,#3987,#3988,#3989,#3990,#3991,#3992,
#3993,#3994,#3995,#3996,#3997,#3998,#3999,#4000));
#4166=CLOSED_SHELL('',(#4001,#4002,#4003,#4004,#4005,#4006,#4007,#4008,
#4009,#4010,#4011,#4012,#4013,#4014,#4015,#4016,#4017,#4018,#4019,#4020,
#4021,#4022,#4023,#4024,#4025,#4026,#4027,#4028,#4029,#4030,#4031,#4032,
#4033,#4034,#4035,#4036,#4037,#4038,#4039,#4040,#4041,#4042,#4043,#4044,
#4045));
#4167=CLOSED_SHELL('',(#4046,#4047,#4048,#4049,#4050,#4051,#4052,#4053));
#4168=CLOSED_SHELL('',(#4054,#4055,#4056,#4057,#4058,#4059,#4060,#4061,
#4062,#4063,#4064,#4065,#4066,#4067,#4068,#4069,#4070,#4071,#4072,#4073,
#4074,#4075,#4076,#4077,#4078,#4079,#4080,#4081,#4082,#4083,#4084,#4085,
#4086,#4087,#4088,#4089,#4090,#4091,#4092,#4093,#4094,#4095,#4096,#4097,
#4098,#4099,#4100,#4101,#4102,#4103,#4104,#4105,#4106,#4107,#4108,#4109,
#4110,#4111,#4112,#4113,#4114,#4115,#4116,#4117,#4118,#4119,#4120,#4121,
#4122,#4123,#4124,#4125,#4126,#4127,#4128,#4129,#4130,#4131,#4132));
#4169=CLOSED_SHELL('',(#4133,#4134,#4135,#4136,#4137,#4138,#4139,#4140));
#4170=CLOSED_SHELL('',(#4141,#4142,#4143,#4144,#4145,#4146,#4147,#4148,
#4149,#4150,#4151,#4152,#4153,#4154,#4155,#4156,#4157,#4158,#4159,#4160,
#4161,#4162,#4163));
#4171=DERIVED_UNIT_ELEMENT(#4185,1.);
#4172=DERIVED_UNIT_ELEMENT(#7785,-3.);
#4173=DERIVED_UNIT_ELEMENT(#4185,1.);
#4174=DERIVED_UNIT_ELEMENT(#7785,-3.);
#4175=DERIVED_UNIT_ELEMENT(#4185,1.);
#4176=DERIVED_UNIT_ELEMENT(#7785,-3.);
#4177=DERIVED_UNIT_ELEMENT(#4185,1.);
#4178=DERIVED_UNIT_ELEMENT(#7785,-3.);
#4179=DERIVED_UNIT_ELEMENT(#4185,1.);
#4180=DERIVED_UNIT_ELEMENT(#7785,-3.);
#4181=DERIVED_UNIT_ELEMENT(#4185,1.);
#4182=DERIVED_UNIT_ELEMENT(#7785,-3.);
#4183=DERIVED_UNIT_ELEMENT(#4185,1.);
#4184=DERIVED_UNIT_ELEMENT(#7785,-3.);
#4185=(
MASS_UNIT()
NAMED_UNIT(*)
SI_UNIT(.KILO.,.GRAM.)
);
#4186=DERIVED_UNIT((#4171,#4172));
#4187=DERIVED_UNIT((#4173,#4174));
#4188=DERIVED_UNIT((#4175,#4176));
#4189=DERIVED_UNIT((#4177,#4178));
#4190=DERIVED_UNIT((#4179,#4180));
#4191=DERIVED_UNIT((#4181,#4182));
#4192=DERIVED_UNIT((#4183,#4184));
#4193=MEASURE_REPRESENTATION_ITEM('density measure',
POSITIVE_RATIO_MEASURE(7850.),#4186);
#4194=MEASURE_REPRESENTATION_ITEM('density measure',
POSITIVE_RATIO_MEASURE(7850.),#4187);
#4195=MEASURE_REPRESENTATION_ITEM('density measure',
POSITIVE_RATIO_MEASURE(7850.),#4188);
#4196=MEASURE_REPRESENTATION_ITEM('density measure',
POSITIVE_RATIO_MEASURE(7850.),#4189);
#4197=MEASURE_REPRESENTATION_ITEM('density measure',
POSITIVE_RATIO_MEASURE(7850.),#4190);
#4198=MEASURE_REPRESENTATION_ITEM('density measure',
POSITIVE_RATIO_MEASURE(7850.),#4191);
#4199=MEASURE_REPRESENTATION_ITEM('density measure',
POSITIVE_RATIO_MEASURE(7850.),#4192);
#4200=PROPERTY_DEFINITION_REPRESENTATION(#4235,#4214);
#4201=PROPERTY_DEFINITION_REPRESENTATION(#4236,#4215);
#4202=PROPERTY_DEFINITION_REPRESENTATION(#4237,#4216);
#4203=PROPERTY_DEFINITION_REPRESENTATION(#4238,#4217);
#4204=PROPERTY_DEFINITION_REPRESENTATION(#4239,#4218);
#4205=PROPERTY_DEFINITION_REPRESENTATION(#4240,#4219);
#4206=PROPERTY_DEFINITION_REPRESENTATION(#4241,#4220);
#4207=PROPERTY_DEFINITION_REPRESENTATION(#4242,#4221);
#4208=PROPERTY_DEFINITION_REPRESENTATION(#4243,#4222);
#4209=PROPERTY_DEFINITION_REPRESENTATION(#4244,#4223);
#4210=PROPERTY_DEFINITION_REPRESENTATION(#4245,#4224);
#4211=PROPERTY_DEFINITION_REPRESENTATION(#4246,#4225);
#4212=PROPERTY_DEFINITION_REPRESENTATION(#4247,#4226);
#4213=PROPERTY_DEFINITION_REPRESENTATION(#4248,#4227);
#4214=REPRESENTATION('material name',(#4228),#7776);
#4215=REPRESENTATION('density',(#4193),#7776);
#4216=REPRESENTATION('material name',(#4229),#7777);
#4217=REPRESENTATION('density',(#4194),#7777);
#4218=REPRESENTATION('material name',(#4230),#7778);
#4219=REPRESENTATION('density',(#4195),#7778);
#4220=REPRESENTATION('material name',(#4231),#7779);
#4221=REPRESENTATION('density',(#4196),#7779);
#4222=REPRESENTATION('material name',(#4232),#7780);
#4223=REPRESENTATION('density',(#4197),#7780);
#4224=REPRESENTATION('material name',(#4233),#7781);
#4225=REPRESENTATION('density',(#4198),#7781);
#4226=REPRESENTATION('material name',(#4234),#7782);
#4227=REPRESENTATION('density',(#4199),#7782);
#4228=DESCRIPTIVE_REPRESENTATION_ITEM('Steel','Steel');
#4229=DESCRIPTIVE_REPRESENTATION_ITEM('Steel','Steel');
#4230=DESCRIPTIVE_REPRESENTATION_ITEM('Steel','Steel');
#4231=DESCRIPTIVE_REPRESENTATION_ITEM('Steel','Steel');
#4232=DESCRIPTIVE_REPRESENTATION_ITEM('Steel','Steel');
#4233=DESCRIPTIVE_REPRESENTATION_ITEM('Steel','Steel');
#4234=DESCRIPTIVE_REPRESENTATION_ITEM('Steel','Steel');
#4235=PROPERTY_DEFINITION('material property','material name',#7830);
#4236=PROPERTY_DEFINITION('material property','density of part',#7830);
#4237=PROPERTY_DEFINITION('material property','material name',#7831);
#4238=PROPERTY_DEFINITION('material property','density of part',#7831);
#4239=PROPERTY_DEFINITION('material property','material name',#7832);
#4240=PROPERTY_DEFINITION('material property','density of part',#7832);
#4241=PROPERTY_DEFINITION('material property','material name',#7833);
#4242=PROPERTY_DEFINITION('material property','density of part',#7833);
#4243=PROPERTY_DEFINITION('material property','material name',#7834);
#4244=PROPERTY_DEFINITION('material property','density of part',#7834);
#4245=PROPERTY_DEFINITION('material property','material name',#7835);
#4246=PROPERTY_DEFINITION('material property','density of part',#7835);
#4247=PROPERTY_DEFINITION('material property','material name',#7836);
#4248=PROPERTY_DEFINITION('material property','density of part',#7836);
#4249=AXIS2_PLACEMENT_3D('',#5997,#4712,#4713);
#4250=AXIS2_PLACEMENT_3D('',#5998,#4714,#4715);
#4251=AXIS2_PLACEMENT_3D('',#5999,#4716,#4717);
#4252=AXIS2_PLACEMENT_3D('',#6000,#4718,#4719);
#4253=AXIS2_PLACEMENT_3D('',#6003,#4720,#4721);
#4254=AXIS2_PLACEMENT_3D('',#6005,#4722,#4723);
#4255=AXIS2_PLACEMENT_3D('',#6007,#4724,#4725);
#4256=AXIS2_PLACEMENT_3D('',#6008,#4726,#4727);
#4257=AXIS2_PLACEMENT_3D('',#6009,#4728,#4729);
#4258=AXIS2_PLACEMENT_3D('',#6011,#4730,#4731);
#4259=AXIS2_PLACEMENT_3D('',#6013,#4732,#4733);
#4260=AXIS2_PLACEMENT_3D('',#6014,#4734,#4735);
#4261=AXIS2_PLACEMENT_3D('',#6015,#4736,#4737);
#4262=AXIS2_PLACEMENT_3D('',#6017,#4738,#4739);
#4263=AXIS2_PLACEMENT_3D('',#6019,#4741,#4742);
#4264=AXIS2_PLACEMENT_3D('',#6021,#4743,#4744);
#4265=AXIS2_PLACEMENT_3D('',#6023,#4745,#4746);
#4266=AXIS2_PLACEMENT_3D('',#6024,#4747,#4748);
#4267=AXIS2_PLACEMENT_3D('',#6025,#4749,#4750);
#4268=AXIS2_PLACEMENT_3D('',#6027,#4751,#4752);
#4269=AXIS2_PLACEMENT_3D('',#6029,#4754,#4755);
#4270=AXIS2_PLACEMENT_3D('',#6032,#4756,#4757);
#4271=AXIS2_PLACEMENT_3D('',#6036,#4759,#4760);
#4272=AXIS2_PLACEMENT_3D('',#6038,#4762,#4763);
#4273=AXIS2_PLACEMENT_3D('',#6040,#4764,#4765);
#4274=AXIS2_PLACEMENT_3D('',#6043,#4767,#4768);
#4275=AXIS2_PLACEMENT_3D('',#6044,#4769,#4770);
#4276=AXIS2_PLACEMENT_3D('',#6046,#4771,#4772);
#4277=AXIS2_PLACEMENT_3D('',#6049,#4774,#4775);
#4278=AXIS2_PLACEMENT_3D('',#6050,#4776,#4777);
#4279=AXIS2_PLACEMENT_3D('',#6053,#4778,#4779);
#4280=AXIS2_PLACEMENT_3D('',#6057,#4781,#4782);
#4281=AXIS2_PLACEMENT_3D('',#6059,#4784,#4785);
#4282=AXIS2_PLACEMENT_3D('',#6062,#4786,#4787);
#4283=AXIS2_PLACEMENT_3D('',#6066,#4789,#4790);
#4284=AXIS2_PLACEMENT_3D('',#6068,#4792,#4793);
#4285=AXIS2_PLACEMENT_3D('',#6071,#4794,#4795);
#4286=AXIS2_PLACEMENT_3D('',#6075,#4797,#4798);
#4287=AXIS2_PLACEMENT_3D('',#6077,#4800,#4801);
#4288=AXIS2_PLACEMENT_3D('',#6080,#4802,#4803);
#4289=AXIS2_PLACEMENT_3D('',#6084,#4805,#4806);
#4290=AXIS2_PLACEMENT_3D('',#6086,#4808,#4809);
#4291=AXIS2_PLACEMENT_3D('',#6089,#4810,#4811);
#4292=AXIS2_PLACEMENT_3D('',#6092,#4814,#4815);
#4293=AXIS2_PLACEMENT_3D('',#6096,#4817,#4818);
#4294=AXIS2_PLACEMENT_3D('',#6098,#4820,#4821);
#4295=AXIS2_PLACEMENT_3D('',#6111,#4827,#4828);
#4296=AXIS2_PLACEMENT_3D('',#6139,#4842,#4843);
#4297=AXIS2_PLACEMENT_3D('',#6143,#4846,#4847);
#4298=AXIS2_PLACEMENT_3D('',#6151,#4854,#4855);
#4299=AXIS2_PLACEMENT_3D('',#6165,#4863,#4864);
#4300=AXIS2_PLACEMENT_3D('',#6171,#4868,#4869);
#4301=AXIS2_PLACEMENT_3D('',#6188,#4880,#4881);
#4302=AXIS2_PLACEMENT_3D('',#6190,#4882,#4883);
#4303=AXIS2_PLACEMENT_3D('',#6192,#4885,#4886);
#4304=AXIS2_PLACEMENT_3D('',#6194,#4888,#4889);
#4305=AXIS2_PLACEMENT_3D('',#6196,#4891,#4892);
#4306=AXIS2_PLACEMENT_3D('',#6198,#4894,#4895);
#4307=AXIS2_PLACEMENT_3D('',#6200,#4897,#4898);
#4308=AXIS2_PLACEMENT_3D('',#6205,#4901,#4902);
#4309=AXIS2_PLACEMENT_3D('',#6214,#4907,#4908);
#4310=AXIS2_PLACEMENT_3D('',#6221,#4913,#4914);
#4311=AXIS2_PLACEMENT_3D('',#6223,#4916,#4917);
#4312=AXIS2_PLACEMENT_3D('',#6225,#4919,#4920);
#4313=AXIS2_PLACEMENT_3D('',#6227,#4922,#4923);
#4314=AXIS2_PLACEMENT_3D('',#6228,#4924,#4925);
#4315=AXIS2_PLACEMENT_3D('',#6231,#4928,#4929);
#4316=AXIS2_PLACEMENT_3D('',#6233,#4931,#4932);
#4317=AXIS2_PLACEMENT_3D('',#6235,#4934,#4935);
#4318=AXIS2_PLACEMENT_3D('',#6237,#4937,#4938);
#4319=AXIS2_PLACEMENT_3D('',#6238,#4939,#4940);
#4320=AXIS2_PLACEMENT_3D('',#6241,#4943,#4944);
#4321=AXIS2_PLACEMENT_3D('',#6242,#4945,#4946);
#4322=AXIS2_PLACEMENT_3D('',#6243,#4947,#4948);
#4323=AXIS2_PLACEMENT_3D('',#6246,#4951,#4952);
#4324=AXIS2_PLACEMENT_3D('',#6247,#4953,#4954);
#4325=AXIS2_PLACEMENT_3D('',#6248,#4955,#4956);
#4326=AXIS2_PLACEMENT_3D('',#6249,#4957,#4958);
#4327=AXIS2_PLACEMENT_3D('',#6250,#4959,#4960);
#4328=AXIS2_PLACEMENT_3D('',#6257,#4965,#4966);
#4329=AXIS2_PLACEMENT_3D('',#6267,#4972,#4973);
#4330=AXIS2_PLACEMENT_3D('',#6270,#4976,#4977);
#4331=AXIS2_PLACEMENT_3D('',#6272,#4979,#4980);
#4332=AXIS2_PLACEMENT_3D('',#6274,#4982,#4983);
#4333=AXIS2_PLACEMENT_3D('',#6275,#4984,#4985);
#4334=AXIS2_PLACEMENT_3D('',#6276,#4986,#4987);
#4335=AXIS2_PLACEMENT_3D('',#6277,#4988,#4989);
#4336=AXIS2_PLACEMENT_3D('',#6278,#4990,#4991);
#4337=AXIS2_PLACEMENT_3D('',#6279,#4992,#4993);
#4338=AXIS2_PLACEMENT_3D('',#6280,#4994,#4995);
#4339=AXIS2_PLACEMENT_3D('',#6281,#4996,#4997);
#4340=AXIS2_PLACEMENT_3D('',#6283,#4998,#4999);
#4341=AXIS2_PLACEMENT_3D('',#6286,#5001,#5002);
#4342=AXIS2_PLACEMENT_3D('',#6287,#5003,#5004);
#4343=AXIS2_PLACEMENT_3D('',#6289,#5005,#5006);
#4344=AXIS2_PLACEMENT_3D('',#6292,#5008,#5009);
#4345=AXIS2_PLACEMENT_3D('',#6293,#5010,#5011);
#4346=AXIS2_PLACEMENT_3D('',#6295,#5012,#5013);
#4347=AXIS2_PLACEMENT_3D('',#6299,#5015,#5016);
#4348=AXIS2_PLACEMENT_3D('',#6301,#5017,#5018);
#4349=AXIS2_PLACEMENT_3D('',#6303,#5019,#5020);
#4350=AXIS2_PLACEMENT_3D('',#6305,#5021,#5022);
#4351=AXIS2_PLACEMENT_3D('',#6307,#5023,#5024);
#4352=AXIS2_PLACEMENT_3D('',#6309,#5025,#5026);
#4353=AXIS2_PLACEMENT_3D('',#6310,#5027,#5028);
#4354=AXIS2_PLACEMENT_3D('',#6311,#5029,#5030);
#4355=AXIS2_PLACEMENT_3D('',#6313,#5031,#5032);
#4356=AXIS2_PLACEMENT_3D('',#6316,#5034,#5035);
#4357=AXIS2_PLACEMENT_3D('',#6317,#5036,#5037);
#4358=AXIS2_PLACEMENT_3D('',#6330,#5044,#5045);
#4359=AXIS2_PLACEMENT_3D('',#6331,#5046,#5047);
#4360=AXIS2_PLACEMENT_3D('',#6337,#5051,#5052);
#4361=AXIS2_PLACEMENT_3D('',#6341,#5055,#5056);
#4362=AXIS2_PLACEMENT_3D('',#6345,#5059,#5060);
#4363=AXIS2_PLACEMENT_3D('',#6349,#5063,#5064);
#4364=AXIS2_PLACEMENT_3D('',#6353,#5067,#5068);
#4365=AXIS2_PLACEMENT_3D('',#6355,#5070,#5071);
#4366=AXIS2_PLACEMENT_3D('',#6356,#5072,#5073);
#4367=AXIS2_PLACEMENT_3D('',#6369,#5080,#5081);
#4368=AXIS2_PLACEMENT_3D('',#6373,#5084,#5085);
#4369=AXIS2_PLACEMENT_3D('',#6377,#5088,#5089);
#4370=AXIS2_PLACEMENT_3D('',#6381,#5092,#5093);
#4371=AXIS2_PLACEMENT_3D('',#6385,#5096,#5097);
#4372=AXIS2_PLACEMENT_3D('',#6389,#5100,#5101);
#4373=AXIS2_PLACEMENT_3D('',#6393,#5104,#5105);
#4374=AXIS2_PLACEMENT_3D('',#6396,#5108,#5109);
#4375=AXIS2_PLACEMENT_3D('',#6398,#5111,#5112);
#4376=AXIS2_PLACEMENT_3D('',#6400,#5114,#5115);
#4377=AXIS2_PLACEMENT_3D('',#6402,#5117,#5118);
#4378=AXIS2_PLACEMENT_3D('',#6404,#5120,#5121);
#4379=AXIS2_PLACEMENT_3D('',#6405,#5122,#5123);
#4380=AXIS2_PLACEMENT_3D('',#6406,#5124,#5125);
#4381=AXIS2_PLACEMENT_3D('',#6407,#5126,#5127);
#4382=AXIS2_PLACEMENT_3D('',#6408,#5128,#5129);
#4383=AXIS2_PLACEMENT_3D('',#6411,#5130,#5131);
#4384=AXIS2_PLACEMENT_3D('',#6415,#5133,#5134);
#4385=AXIS2_PLACEMENT_3D('',#6417,#5136,#5137);
#4386=AXIS2_PLACEMENT_3D('',#6420,#5138,#5139);
#4387=AXIS2_PLACEMENT_3D('',#6424,#5141,#5142);
#4388=AXIS2_PLACEMENT_3D('',#6426,#5144,#5145);
#4389=AXIS2_PLACEMENT_3D('',#6429,#5146,#5147);
#4390=AXIS2_PLACEMENT_3D('',#6433,#5149,#5150);
#4391=AXIS2_PLACEMENT_3D('',#6435,#5152,#5153);
#4392=AXIS2_PLACEMENT_3D('',#6437,#5154,#5155);
#4393=AXIS2_PLACEMENT_3D('',#6440,#5157,#5158);
#4394=AXIS2_PLACEMENT_3D('',#6441,#5159,#5160);
#4395=AXIS2_PLACEMENT_3D('',#6443,#5161,#5162);
#4396=AXIS2_PLACEMENT_3D('',#6446,#5164,#5165);
#4397=AXIS2_PLACEMENT_3D('',#6447,#5166,#5167);
#4398=AXIS2_PLACEMENT_3D('',#6449,#5168,#5169);
#4399=AXIS2_PLACEMENT_3D('',#6452,#5171,#5172);
#4400=AXIS2_PLACEMENT_3D('',#6453,#5173,#5174);
#4401=AXIS2_PLACEMENT_3D('',#6455,#5175,#5176);
#4402=AXIS2_PLACEMENT_3D('',#6456,#5177,#5178);
#4403=AXIS2_PLACEMENT_3D('',#6458,#5179,#5180);
#4404=AXIS2_PLACEMENT_3D('',#6460,#5182,#5183);
#4405=AXIS2_PLACEMENT_3D('',#6462,#5184,#5185);
#4406=AXIS2_PLACEMENT_3D('',#6465,#5187,#5188);
#4407=AXIS2_PLACEMENT_3D('',#6466,#5189,#5190);
#4408=AXIS2_PLACEMENT_3D('',#6468,#5191,#5192);
#4409=AXIS2_PLACEMENT_3D('',#6471,#5194,#5195);
#4410=AXIS2_PLACEMENT_3D('',#6472,#5196,#5197);
#4411=AXIS2_PLACEMENT_3D('',#6473,#5198,#5199);
#4412=AXIS2_PLACEMENT_3D('',#6475,#5200,#5201);
#4413=AXIS2_PLACEMENT_3D('',#6478,#5203,#5204);
#4414=AXIS2_PLACEMENT_3D('',#6479,#5205,#5206);
#4415=AXIS2_PLACEMENT_3D('',#6481,#5207,#5208);
#4416=AXIS2_PLACEMENT_3D('',#6484,#5210,#5211);
#4417=AXIS2_PLACEMENT_3D('',#6485,#5212,#5213);
#4418=AXIS2_PLACEMENT_3D('',#6487,#5214,#5215);
#4419=AXIS2_PLACEMENT_3D('',#6490,#5217,#5218);
#4420=AXIS2_PLACEMENT_3D('',#6491,#5219,#5220);
#4421=AXIS2_PLACEMENT_3D('',#6492,#5221,#5222);
#4422=AXIS2_PLACEMENT_3D('',#6494,#5224,#5225);
#4423=AXIS2_PLACEMENT_3D('',#6496,#5227,#5228);
#4424=AXIS2_PLACEMENT_3D('',#6537,#5249,#5250);
#4425=AXIS2_PLACEMENT_3D('',#6578,#5271,#5272);
#4426=AXIS2_PLACEMENT_3D('',#6579,#5273,#5274);
#4427=AXIS2_PLACEMENT_3D('',#6581,#5276,#5277);
#4428=AXIS2_PLACEMENT_3D('',#6582,#5278,#5279);
#4429=AXIS2_PLACEMENT_3D('',#6584,#5281,#5282);
#4430=AXIS2_PLACEMENT_3D('',#6585,#5283,#5284);
#4431=AXIS2_PLACEMENT_3D('',#6587,#5286,#5287);
#4432=AXIS2_PLACEMENT_3D('',#6588,#5288,#5289);
#4433=AXIS2_PLACEMENT_3D('',#6590,#5291,#5292);
#4434=AXIS2_PLACEMENT_3D('',#6591,#5293,#5294);
#4435=AXIS2_PLACEMENT_3D('',#6593,#5296,#5297);
#4436=AXIS2_PLACEMENT_3D('',#6594,#5298,#5299);
#4437=AXIS2_PLACEMENT_3D('',#6596,#5301,#5302);
#4438=AXIS2_PLACEMENT_3D('',#6597,#5303,#5304);
#4439=AXIS2_PLACEMENT_3D('',#6599,#5306,#5307);
#4440=AXIS2_PLACEMENT_3D('',#6600,#5308,#5309);
#4441=AXIS2_PLACEMENT_3D('',#6602,#5311,#5312);
#4442=AXIS2_PLACEMENT_3D('',#6604,#5314,#5315);
#4443=AXIS2_PLACEMENT_3D('',#6606,#5317,#5318);
#4444=AXIS2_PLACEMENT_3D('',#6607,#5319,#5320);
#4445=AXIS2_PLACEMENT_3D('',#6608,#5321,#5322);
#4446=AXIS2_PLACEMENT_3D('',#6610,#5324,#5325);
#4447=AXIS2_PLACEMENT_3D('',#6612,#5327,#5328);
#4448=AXIS2_PLACEMENT_3D('',#6613,#5329,#5330);
#4449=AXIS2_PLACEMENT_3D('',#6614,#5331,#5332);
#4450=AXIS2_PLACEMENT_3D('',#6615,#5333,#5334);
#4451=AXIS2_PLACEMENT_3D('',#6616,#5335,#5336);
#4452=AXIS2_PLACEMENT_3D('',#6617,#5337,#5338);
#4453=AXIS2_PLACEMENT_3D('',#6618,#5339,#5340);
#4454=AXIS2_PLACEMENT_3D('',#6619,#5341,#5342);
#4455=AXIS2_PLACEMENT_3D('',#6620,#5343,#5344);
#4456=AXIS2_PLACEMENT_3D('',#6621,#5345,#5346);
#4457=AXIS2_PLACEMENT_3D('',#6622,#5347,#5348);
#4458=AXIS2_PLACEMENT_3D('',#6625,#5351,#5352);
#4459=AXIS2_PLACEMENT_3D('',#6628,#5355,#5356);
#4460=AXIS2_PLACEMENT_3D('',#6629,#5357,#5358);
#4461=AXIS2_PLACEMENT_3D('',#6630,#5359,#5360);
#4462=AXIS2_PLACEMENT_3D('',#6631,#5361,#5362);
#4463=AXIS2_PLACEMENT_3D('',#6633,#5363,#5364);
#4464=AXIS2_PLACEMENT_3D('',#6636,#5366,#5367);
#4465=AXIS2_PLACEMENT_3D('',#6637,#5368,#5369);
#4466=AXIS2_PLACEMENT_3D('',#6639,#5370,#5371);
#4467=AXIS2_PLACEMENT_3D('',#6642,#5373,#5374);
#4468=AXIS2_PLACEMENT_3D('',#6643,#5375,#5376);
#4469=AXIS2_PLACEMENT_3D('',#6646,#5377,#5378);
#4470=AXIS2_PLACEMENT_3D('',#6650,#5380,#5381);
#4471=AXIS2_PLACEMENT_3D('',#6652,#5383,#5384);
#4472=AXIS2_PLACEMENT_3D('',#6656,#5386,#5387);
#4473=AXIS2_PLACEMENT_3D('',#6658,#5389,#5390);
#4474=AXIS2_PLACEMENT_3D('',#6662,#5392,#5393);
#4475=AXIS2_PLACEMENT_3D('',#6664,#5395,#5396);
#4476=AXIS2_PLACEMENT_3D('',#6666,#5398,#5399);
#4477=AXIS2_PLACEMENT_3D('',#6668,#5401,#5402);
#4478=AXIS2_PLACEMENT_3D('',#6669,#5403,#5404);
#4479=AXIS2_PLACEMENT_3D('',#6670,#5405,#5406);
#4480=AXIS2_PLACEMENT_3D('',#6672,#5407,#5408);
#4481=AXIS2_PLACEMENT_3D('',#6675,#5410,#5411);
#4482=AXIS2_PLACEMENT_3D('',#6676,#5412,#5413);
#4483=AXIS2_PLACEMENT_3D('',#6678,#5414,#5415);
#4484=AXIS2_PLACEMENT_3D('',#6681,#5417,#5418);
#4485=AXIS2_PLACEMENT_3D('',#6682,#5419,#5420);
#4486=AXIS2_PLACEMENT_3D('',#6685,#5421,#5422);
#4487=AXIS2_PLACEMENT_3D('',#6686,#5423,#5424);
#4488=AXIS2_PLACEMENT_3D('',#6689,#5426,#5427);
#4489=AXIS2_PLACEMENT_3D('',#6690,#5428,#5429);
#4490=AXIS2_PLACEMENT_3D('',#6693,#5430,#5431);
#4491=AXIS2_PLACEMENT_3D('',#6694,#5432,#5433);
#4492=AXIS2_PLACEMENT_3D('',#6697,#5435,#5436);
#4493=AXIS2_PLACEMENT_3D('',#6698,#5437,#5438);
#4494=AXIS2_PLACEMENT_3D('',#6700,#5439,#5440);
#4495=AXIS2_PLACEMENT_3D('',#6702,#5442,#5443);
#4496=AXIS2_PLACEMENT_3D('',#6705,#5445,#5446);
#4497=AXIS2_PLACEMENT_3D('',#6706,#5447,#5448);
#4498=AXIS2_PLACEMENT_3D('',#6708,#5449,#5450);
#4499=AXIS2_PLACEMENT_3D('',#6711,#5452,#5453);
#4500=AXIS2_PLACEMENT_3D('',#6712,#5454,#5455);
#4501=AXIS2_PLACEMENT_3D('',#6714,#5456,#5457);
#4502=AXIS2_PLACEMENT_3D('',#6716,#5459,#5460);
#4503=AXIS2_PLACEMENT_3D('',#6719,#5462,#5463);
#4504=AXIS2_PLACEMENT_3D('',#6720,#5464,#5465);
#4505=AXIS2_PLACEMENT_3D('',#6723,#5466,#5467);
#4506=AXIS2_PLACEMENT_3D('',#6725,#5468,#5469);
#4507=AXIS2_PLACEMENT_3D('',#6727,#5470,#5471);
#4508=AXIS2_PLACEMENT_3D('',#6728,#5472,#5473);
#4509=AXIS2_PLACEMENT_3D('',#6729,#5474,#5475);
#4510=AXIS2_PLACEMENT_3D('',#6732,#5476,#5477);
#4511=AXIS2_PLACEMENT_3D('',#6734,#5478,#5479);
#4512=AXIS2_PLACEMENT_3D('',#6736,#5480,#5481);
#4513=AXIS2_PLACEMENT_3D('',#6738,#5482,#5483);
#4514=AXIS2_PLACEMENT_3D('',#6739,#5484,#5485);
#4515=AXIS2_PLACEMENT_3D('',#6740,#5486,#5487);
#4516=AXIS2_PLACEMENT_3D('',#6743,#5488,#5489);
#4517=AXIS2_PLACEMENT_3D('',#6745,#5490,#5491);
#4518=AXIS2_PLACEMENT_3D('',#6747,#5492,#5493);
#4519=AXIS2_PLACEMENT_3D('',#6748,#5494,#5495);
#4520=AXIS2_PLACEMENT_3D('',#6749,#5496,#5497);
#4521=AXIS2_PLACEMENT_3D('',#6751,#5498,#5499);
#4522=AXIS2_PLACEMENT_3D('',#6754,#5501,#5502);
#4523=AXIS2_PLACEMENT_3D('',#6755,#5503,#5504);
#4524=AXIS2_PLACEMENT_3D('',#6759,#5506,#5507);
#4525=AXIS2_PLACEMENT_3D('',#6761,#5509,#5510);
#4526=AXIS2_PLACEMENT_3D('',#6763,#5511,#5512);
#4527=AXIS2_PLACEMENT_3D('',#6766,#5514,#5515);
#4528=AXIS2_PLACEMENT_3D('',#6767,#5516,#5517);
#4529=AXIS2_PLACEMENT_3D('',#6770,#5518,#5519);
#4530=AXIS2_PLACEMENT_3D('',#6774,#5521,#5522);
#4531=AXIS2_PLACEMENT_3D('',#6776,#5524,#5525);
#4532=AXIS2_PLACEMENT_3D('',#6778,#5526,#5527);
#4533=AXIS2_PLACEMENT_3D('',#6782,#5529,#5530);
#4534=AXIS2_PLACEMENT_3D('',#6900,#5533,#5534);
#4535=AXIS2_PLACEMENT_3D('',#7036,#5536,#5537);
#4536=AXIS2_PLACEMENT_3D('',#7037,#5538,#5539);
#4537=AXIS2_PLACEMENT_3D('',#7041,#5541,#5542);
#4538=AXIS2_PLACEMENT_3D('',#7045,#5544,#5545);
#4539=AXIS2_PLACEMENT_3D('',#7051,#5549,#5550);
#4540=AXIS2_PLACEMENT_3D('',#7059,#5556,#5557);
#4541=AXIS2_PLACEMENT_3D('',#7070,#5564,#5565);
#4542=AXIS2_PLACEMENT_3D('',#7074,#5567,#5568);
#4543=AXIS2_PLACEMENT_3D('',#7075,#5569,#5570);
#4544=AXIS2_PLACEMENT_3D('',#7076,#5571,#5572);
#4545=AXIS2_PLACEMENT_3D('',#7082,#5575,#5576);
#4546=AXIS2_PLACEMENT_3D('',#7086,#5578,#5579);
#4547=AXIS2_PLACEMENT_3D('',#7091,#5582,#5583);
#4548=AXIS2_PLACEMENT_3D('',#7095,#5585,#5586);
#4549=AXIS2_PLACEMENT_3D('',#7105,#5592,#5593);
#4550=AXIS2_PLACEMENT_3D('',#7108,#5594,#5595);
#4551=AXIS2_PLACEMENT_3D('',#7123,#5603,#5604);
#4552=AXIS2_PLACEMENT_3D('',#7127,#5606,#5607);
#4553=AXIS2_PLACEMENT_3D('',#7132,#5610,#5611);
#4554=AXIS2_PLACEMENT_3D('',#7134,#5613,#5614);
#4555=AXIS2_PLACEMENT_3D('',#7140,#5618,#5619);
#4556=AXIS2_PLACEMENT_3D('',#7141,#5620,#5621);
#4557=AXIS2_PLACEMENT_3D('',#7142,#5622,#5623);
#4558=AXIS2_PLACEMENT_3D('',#7145,#5626,#5627);
#4559=AXIS2_PLACEMENT_3D('',#7146,#5628,#5629);
#4560=AXIS2_PLACEMENT_3D('',#7149,#5632,#5633);
#4561=AXIS2_PLACEMENT_3D('',#7150,#5634,#5635);
#4562=AXIS2_PLACEMENT_3D('',#7159,#5640,#5641);
#4563=AXIS2_PLACEMENT_3D('',#7160,#5642,#5643);
#4564=AXIS2_PLACEMENT_3D('',#7166,#5646,#5647);
#4565=AXIS2_PLACEMENT_3D('',#7173,#5651,#5652);
#4566=AXIS2_PLACEMENT_3D('',#7174,#5653,#5654);
#4567=AXIS2_PLACEMENT_3D('',#7177,#5655,#5656);
#4568=AXIS2_PLACEMENT_3D('',#7183,#5660,#5661);
#4569=AXIS2_PLACEMENT_3D('',#7184,#5662,#5663);
#4570=AXIS2_PLACEMENT_3D('',#7185,#5664,#5665);
#4571=AXIS2_PLACEMENT_3D('',#7186,#5666,#5667);
#4572=AXIS2_PLACEMENT_3D('',#7187,#5668,#5669);
#4573=AXIS2_PLACEMENT_3D('',#7188,#5670,#5671);
#4574=AXIS2_PLACEMENT_3D('',#7197,#5676,#5677);
#4575=AXIS2_PLACEMENT_3D('',#7198,#5678,#5679);
#4576=AXIS2_PLACEMENT_3D('',#7199,#5680,#5681);
#4577=AXIS2_PLACEMENT_3D('',#7200,#5682,#5683);
#4578=AXIS2_PLACEMENT_3D('',#7201,#5684,#5685);
#4579=AXIS2_PLACEMENT_3D('',#7202,#5686,#5687);
#4580=AXIS2_PLACEMENT_3D('',#7203,#5688,#5689);
#4581=AXIS2_PLACEMENT_3D('',#7204,#5690,#5691);
#4582=AXIS2_PLACEMENT_3D('',#7205,#5692,#5693);
#4583=AXIS2_PLACEMENT_3D('',#7206,#5694,#5695);
#4584=AXIS2_PLACEMENT_3D('',#7207,#5696,#5697);
#4585=AXIS2_PLACEMENT_3D('',#7208,#5698,#5699);
#4586=AXIS2_PLACEMENT_3D('',#7209,#5700,#5701);
#4587=AXIS2_PLACEMENT_3D('',#7210,#5702,#5703);
#4588=AXIS2_PLACEMENT_3D('',#7211,#5704,#5705);
#4589=AXIS2_PLACEMENT_3D('',#7212,#5706,#5707);
#4590=AXIS2_PLACEMENT_3D('',#7213,#5708,#5709);
#4591=AXIS2_PLACEMENT_3D('',#7214,#5710,#5711);
#4592=AXIS2_PLACEMENT_3D('',#7215,#5712,#5713);
#4593=AXIS2_PLACEMENT_3D('',#7216,#5714,#5715);
#4594=AXIS2_PLACEMENT_3D('',#7217,#5716,#5717);
#4595=AXIS2_PLACEMENT_3D('',#7218,#5718,#5719);
#4596=AXIS2_PLACEMENT_3D('',#7219,#5720,#5721);
#4597=AXIS2_PLACEMENT_3D('',#7220,#5722,#5723);
#4598=AXIS2_PLACEMENT_3D('',#7221,#5724,#5725);
#4599=AXIS2_PLACEMENT_3D('',#7222,#5726,#5727);
#4600=AXIS2_PLACEMENT_3D('',#7223,#5728,#5729);
#4601=AXIS2_PLACEMENT_3D('',#7240,#5730,#5731);
#4602=AXIS2_PLACEMENT_3D('',#7241,#5732,#5733);
#4603=AXIS2_PLACEMENT_3D('',#7284,#5734,#5735);
#4604=AXIS2_PLACEMENT_3D('',#7285,#5736,#5737);
#4605=AXIS2_PLACEMENT_3D('',#7286,#5738,#5739);
#4606=AXIS2_PLACEMENT_3D('',#7287,#5740,#5741);
#4607=AXIS2_PLACEMENT_3D('',#7346,#5742,#5743);
#4608=AXIS2_PLACEMENT_3D('',#7347,#5744,#5745);
#4609=AXIS2_PLACEMENT_3D('',#7348,#5746,#5747);
#4610=AXIS2_PLACEMENT_3D('',#7349,#5748,#5749);
#4611=AXIS2_PLACEMENT_3D('',#7350,#5750,#5751);
#4612=AXIS2_PLACEMENT_3D('',#7351,#5752,#5753);
#4613=AXIS2_PLACEMENT_3D('',#7352,#5754,#5755);
#4614=AXIS2_PLACEMENT_3D('',#7353,#5756,#5757);
#4615=AXIS2_PLACEMENT_3D('',#7354,#5758,#5759);
#4616=AXIS2_PLACEMENT_3D('',#7355,#5760,#5761);
#4617=AXIS2_PLACEMENT_3D('',#7356,#5762,#5763);
#4618=AXIS2_PLACEMENT_3D('',#7357,#5764,#5765);
#4619=AXIS2_PLACEMENT_3D('',#7358,#5766,#5767);
#4620=AXIS2_PLACEMENT_3D('',#7359,#5768,#5769);
#4621=AXIS2_PLACEMENT_3D('',#7360,#5770,#5771);
#4622=AXIS2_PLACEMENT_3D('',#7361,#5772,#5773);
#4623=AXIS2_PLACEMENT_3D('',#7362,#5774,#5775);
#4624=AXIS2_PLACEMENT_3D('',#7363,#5776,#5777);
#4625=AXIS2_PLACEMENT_3D('',#7364,#5778,#5779);
#4626=AXIS2_PLACEMENT_3D('',#7365,#5780,#5781);
#4627=AXIS2_PLACEMENT_3D('',#7366,#5782,#5783);
#4628=AXIS2_PLACEMENT_3D('',#7367,#5784,#5785);
#4629=AXIS2_PLACEMENT_3D('',#7368,#5786,#5787);
#4630=AXIS2_PLACEMENT_3D('',#7369,#5788,#5789);
#4631=AXIS2_PLACEMENT_3D('',#7370,#5790,#5791);
#4632=AXIS2_PLACEMENT_3D('',#7371,#5792,#5793);
#4633=AXIS2_PLACEMENT_3D('',#7442,#5794,#5795);
#4634=AXIS2_PLACEMENT_3D('',#7443,#5796,#5797);
#4635=AXIS2_PLACEMENT_3D('',#7486,#5798,#5799);
#4636=AXIS2_PLACEMENT_3D('',#7487,#5800,#5801);
#4637=AXIS2_PLACEMENT_3D('',#7488,#5802,#5803);
#4638=AXIS2_PLACEMENT_3D('',#7489,#5804,#5805);
#4639=AXIS2_PLACEMENT_3D('',#7490,#5806,#5807);
#4640=AXIS2_PLACEMENT_3D('',#7491,#5808,#5809);
#4641=AXIS2_PLACEMENT_3D('',#7604,#5810,#5811);
#4642=AXIS2_PLACEMENT_3D('',#7605,#5812,#5813);
#4643=AXIS2_PLACEMENT_3D('',#7606,#5814,#5815);
#4644=AXIS2_PLACEMENT_3D('',#7607,#5816,#5817);
#4645=AXIS2_PLACEMENT_3D('',#7608,#5818,#5819);
#4646=AXIS2_PLACEMENT_3D('',#7609,#5820,#5821);
#4647=AXIS2_PLACEMENT_3D('',#7610,#5822,#5823);
#4648=AXIS2_PLACEMENT_3D('',#7612,#5824,#5825);
#4649=AXIS2_PLACEMENT_3D('',#7615,#5827,#5828);
#4650=AXIS2_PLACEMENT_3D('',#7616,#5829,#5830);
#4651=AXIS2_PLACEMENT_3D('',#7618,#5831,#5832);
#4652=AXIS2_PLACEMENT_3D('',#7621,#5834,#5835);
#4653=AXIS2_PLACEMENT_3D('',#7622,#5836,#5837);
#4654=AXIS2_PLACEMENT_3D('',#7625,#5838,#5839);
#4655=AXIS2_PLACEMENT_3D('',#7629,#5841,#5842);
#4656=AXIS2_PLACEMENT_3D('',#7631,#5844,#5845);
#4657=AXIS2_PLACEMENT_3D('',#7635,#5847,#5848);
#4658=AXIS2_PLACEMENT_3D('',#7637,#5850,#5851);
#4659=AXIS2_PLACEMENT_3D('',#7641,#5853,#5854);
#4660=AXIS2_PLACEMENT_3D('',#7643,#5856,#5857);
#4661=AXIS2_PLACEMENT_3D('',#7645,#5859,#5860);
#4662=AXIS2_PLACEMENT_3D('',#7647,#5862,#5863);
#4663=AXIS2_PLACEMENT_3D('',#7648,#5864,#5865);
#4664=AXIS2_PLACEMENT_3D('',#7649,#5866,#5867);
#4665=AXIS2_PLACEMENT_3D('',#7652,#5868,#5869);
#4666=AXIS2_PLACEMENT_3D('',#7653,#5870,#5871);
#4667=AXIS2_PLACEMENT_3D('',#7656,#5873,#5874);
#4668=AXIS2_PLACEMENT_3D('',#7657,#5875,#5876);
#4669=AXIS2_PLACEMENT_3D('',#7660,#5877,#5878);
#4670=AXIS2_PLACEMENT_3D('',#7661,#5879,#5880);
#4671=AXIS2_PLACEMENT_3D('',#7664,#5882,#5883);
#4672=AXIS2_PLACEMENT_3D('',#7665,#5884,#5885);
#4673=AXIS2_PLACEMENT_3D('',#7667,#5886,#5887);
#4674=AXIS2_PLACEMENT_3D('',#7670,#5889,#5890);
#4675=AXIS2_PLACEMENT_3D('',#7671,#5891,#5892);
#4676=AXIS2_PLACEMENT_3D('',#7673,#5893,#5894);
#4677=AXIS2_PLACEMENT_3D('',#7676,#5896,#5897);
#4678=AXIS2_PLACEMENT_3D('',#7677,#5898,#5899);
#4679=AXIS2_PLACEMENT_3D('',#7679,#5900,#5901);
#4680=AXIS2_PLACEMENT_3D('',#7681,#5903,#5904);
#4681=AXIS2_PLACEMENT_3D('',#7684,#5906,#5907);
#4682=AXIS2_PLACEMENT_3D('',#7685,#5908,#5909);
#4683=AXIS2_PLACEMENT_3D('',#7687,#5910,#5911);
#4684=AXIS2_PLACEMENT_3D('',#7689,#5913,#5914);
#4685=AXIS2_PLACEMENT_3D('',#7692,#5916,#5917);
#4686=AXIS2_PLACEMENT_3D('',#7693,#5918,#5919);
#4687=AXIS2_PLACEMENT_3D('',#7712,#5929,#5930);
#4688=AXIS2_PLACEMENT_3D('',#7731,#5940,#5941);
#4689=AXIS2_PLACEMENT_3D('',#7734,#5944,#5945);
#4690=AXIS2_PLACEMENT_3D('',#7736,#5947,#5948);
#4691=AXIS2_PLACEMENT_3D('',#7738,#5950,#5951);
#4692=AXIS2_PLACEMENT_3D('',#7740,#5953,#5954);
#4693=AXIS2_PLACEMENT_3D('',#7742,#5956,#5957);
#4694=AXIS2_PLACEMENT_3D('',#7744,#5959,#5960);
#4695=AXIS2_PLACEMENT_3D('',#7746,#5962,#5963);
#4696=AXIS2_PLACEMENT_3D('',#7748,#5965,#5966);
#4697=AXIS2_PLACEMENT_3D('',#7749,#5967,#5968);
#4698=AXIS2_PLACEMENT_3D('',#7750,#5969,#5970);
#4699=AXIS2_PLACEMENT_3D('',#7751,#5971,#5972);
#4700=AXIS2_PLACEMENT_3D('',#7752,#5973,#5974);
#4701=AXIS2_PLACEMENT_3D('',#7753,#5975,#5976);
#4702=AXIS2_PLACEMENT_3D('',#7754,#5977,#5978);
#4703=AXIS2_PLACEMENT_3D('',#7755,#5979,#5980);
#4704=AXIS2_PLACEMENT_3D('',#7756,#5981,#5982);
#4705=AXIS2_PLACEMENT_3D('',#7757,#5983,#5984);
#4706=AXIS2_PLACEMENT_3D('',#7758,#5985,#5986);
#4707=AXIS2_PLACEMENT_3D('',#7759,#5987,#5988);
#4708=AXIS2_PLACEMENT_3D('',#7760,#5989,#5990);
#4709=AXIS2_PLACEMENT_3D('',#7761,#5991,#5992);
#4710=AXIS2_PLACEMENT_3D('',#7762,#5993,#5994);
#4711=AXIS2_PLACEMENT_3D('',#7763,#5995,#5996);
#4712=DIRECTION('axis',(0.,0.,1.));
#4713=DIRECTION('refdir',(1.,0.,0.));
#4714=DIRECTION('axis',(0.,0.,1.));
#4715=DIRECTION('refdir',(1.,0.,0.));
#4716=DIRECTION('axis',(0.,0.,1.));
#4717=DIRECTION('refdir',(1.,0.,0.));
#4718=DIRECTION('center_axis',(0.,0.,1.));
#4719=DIRECTION('ref_axis',(1.,0.,0.));
#4720=DIRECTION('center_axis',(-1.,0.,0.));
#4721=DIRECTION('ref_axis',(0.,0.,-1.));
#4722=DIRECTION('center_axis',(0.,0.,1.));
#4723=DIRECTION('ref_axis',(1.,0.,0.));
#4724=DIRECTION('center_axis',(-1.,0.,0.));
#4725=DIRECTION('ref_axis',(0.,-1.73472347597681E-15,-1.));
#4726=DIRECTION('center_axis',(0.,0.,1.));
#4727=DIRECTION('ref_axis',(1.,0.,0.));
#4728=DIRECTION('center_axis',(-1.,0.,0.));
#4729=DIRECTION('ref_axis',(0.,0.,1.));
#4730=DIRECTION('center_axis',(-1.,0.,0.));
#4731=DIRECTION('ref_axis',(0.,0.,1.));
#4732=DIRECTION('center_axis',(0.,-1.,0.));
#4733=DIRECTION('ref_axis',(0.,0.,-1.));
#4734=DIRECTION('center_axis',(1.,0.,0.));
#4735=DIRECTION('ref_axis',(0.,0.,1.));
#4736=DIRECTION('center_axis',(-1.,0.,0.));
#4737=DIRECTION('ref_axis',(0.,0.,1.));
#4738=DIRECTION('center_axis',(-1.,0.,0.));
#4739=DIRECTION('ref_axis',(0.,0.,-1.));
#4740=DIRECTION('',(1.,0.,0.));
#4741=DIRECTION('center_axis',(-1.,0.,0.));
#4742=DIRECTION('ref_axis',(0.,0.,1.));
#4743=DIRECTION('center_axis',(-1.,0.,0.));
#4744=DIRECTION('ref_axis',(0.,0.,1.));
#4745=DIRECTION('center_axis',(0.,-1.,0.));
#4746=DIRECTION('ref_axis',(0.,0.,-1.));
#4747=DIRECTION('center_axis',(1.,0.,0.));
#4748=DIRECTION('ref_axis',(0.,0.,1.));
#4749=DIRECTION('center_axis',(-1.,0.,0.));
#4750=DIRECTION('ref_axis',(0.,0.,1.));
#4751=DIRECTION('center_axis',(1.,0.,0.));
#4752=DIRECTION('ref_axis',(0.,0.,-1.));
#4753=DIRECTION('',(1.,0.,0.));
#4754=DIRECTION('center_axis',(0.,0.,1.));
#4755=DIRECTION('ref_axis',(1.,0.,0.));
#4756=DIRECTION('center_axis',(0.,0.,-1.));
#4757=DIRECTION('ref_axis',(-1.,0.,0.));
#4758=DIRECTION('',(0.,0.,-1.));
#4759=DIRECTION('center_axis',(0.,0.,-1.));
#4760=DIRECTION('ref_axis',(-1.,0.,0.));
#4761=DIRECTION('',(0.,0.,1.));
#4762=DIRECTION('center_axis',(-1.,0.,0.));
#4763=DIRECTION('ref_axis',(0.,0.,1.));
#4764=DIRECTION('center_axis',(1.,0.,0.));
#4765=DIRECTION('ref_axis',(0.,0.,1.));
#4766=DIRECTION('',(-1.,0.,0.));
#4767=DIRECTION('center_axis',(1.,0.,0.));
#4768=DIRECTION('ref_axis',(0.,0.,1.));
#4769=DIRECTION('center_axis',(-1.,0.,0.));
#4770=DIRECTION('ref_axis',(0.,0.,1.));
#4771=DIRECTION('center_axis',(1.,0.,0.));
#4772=DIRECTION('ref_axis',(0.,0.,-1.));
#4773=DIRECTION('',(-1.,0.,0.));
#4774=DIRECTION('center_axis',(1.,0.,0.));
#4775=DIRECTION('ref_axis',(0.,0.,-1.));
#4776=DIRECTION('center_axis',(0.,0.,1.));
#4777=DIRECTION('ref_axis',(1.,0.,0.));
#4778=DIRECTION('center_axis',(0.,0.,1.));
#4779=DIRECTION('ref_axis',(1.,0.,0.));
#4780=DIRECTION('',(0.,0.,1.));
#4781=DIRECTION('center_axis',(0.,0.,1.));
#4782=DIRECTION('ref_axis',(1.,0.,0.));
#4783=DIRECTION('',(0.,0.,-1.));
#4784=DIRECTION('center_axis',(0.,0.,1.));
#4785=DIRECTION('ref_axis',(1.,0.,0.));
#4786=DIRECTION('center_axis',(0.,0.,1.));
#4787=DIRECTION('ref_axis',(1.,0.,0.));
#4788=DIRECTION('',(0.,0.,1.));
#4789=DIRECTION('center_axis',(0.,0.,1.));
#4790=DIRECTION('ref_axis',(1.,0.,0.));
#4791=DIRECTION('',(0.,0.,-1.));
#4792=DIRECTION('center_axis',(0.,0.,1.));
#4793=DIRECTION('ref_axis',(1.,0.,0.));
#4794=DIRECTION('center_axis',(0.,0.,1.));
#4795=DIRECTION('ref_axis',(1.,0.,0.));
#4796=DIRECTION('',(0.,0.,1.));
#4797=DIRECTION('center_axis',(0.,0.,1.));
#4798=DIRECTION('ref_axis',(1.,0.,0.));
#4799=DIRECTION('',(0.,0.,-1.));
#4800=DIRECTION('center_axis',(0.,0.,1.));
#4801=DIRECTION('ref_axis',(1.,0.,0.));
#4802=DIRECTION('center_axis',(0.,0.,1.));
#4803=DIRECTION('ref_axis',(1.,0.,0.));
#4804=DIRECTION('',(0.,0.,1.));
#4805=DIRECTION('center_axis',(0.,0.,1.));
#4806=DIRECTION('ref_axis',(1.,0.,0.));
#4807=DIRECTION('',(0.,0.,-1.));
#4808=DIRECTION('center_axis',(0.,0.,1.));
#4809=DIRECTION('ref_axis',(1.,0.,0.));
#4810=DIRECTION('center_axis',(0.,0.,1.));
#4811=DIRECTION('ref_axis',(1.,0.,0.));
#4812=DIRECTION('',(0.,0.,1.));
#4813=DIRECTION('',(0.,0.,-1.));
#4814=DIRECTION('center_axis',(0.,0.,1.));
#4815=DIRECTION('ref_axis',(1.,0.,0.));
#4816=DIRECTION('',(0.,0.,1.));
#4817=DIRECTION('center_axis',(0.,0.,1.));
#4818=DIRECTION('ref_axis',(1.,0.,0.));
#4819=DIRECTION('',(0.,0.,-1.));
#4820=DIRECTION('center_axis',(1.,0.,0.));
#4821=DIRECTION('ref_axis',(0.,0.,-1.));
#4822=DIRECTION('',(0.,0.,-1.));
#4823=DIRECTION('',(-8.67361737988404E-17,-1.,0.));
#4824=DIRECTION('',(0.,0.,-1.));
#4825=DIRECTION('',(0.,1.,0.));
#4826=DIRECTION('',(0.,0.672272926960032,0.740303391641961));
#4827=DIRECTION('center_axis',(1.,0.,0.));
#4828=DIRECTION('ref_axis',(0.,0.,1.));
#4829=DIRECTION('',(0.,-0.669715115850366,0.742618114242799));
#4830=DIRECTION('',(0.,0.,1.));
#4831=DIRECTION('',(0.,-1.,0.));
#4832=DIRECTION('',(0.,0.,1.));
#4833=DIRECTION('',(0.,-1.,0.));
#4834=DIRECTION('',(0.,0.,1.));
#4835=DIRECTION('',(0.,-1.,0.));
#4836=DIRECTION('',(0.,0.,1.));
#4837=DIRECTION('',(0.,1.,0.));
#4838=DIRECTION('',(0.,0.,1.));
#4839=DIRECTION('',(0.,-1.,0.));
#4840=DIRECTION('',(0.,0.,-1.));
#4841=DIRECTION('',(0.,-0.669715115850366,-0.742618114242799));
#4842=DIRECTION('center_axis',(1.,0.,0.));
#4843=DIRECTION('ref_axis',(0.,0.,-1.));
#4844=DIRECTION('',(0.,0.672272926960032,-0.740303391641961));
#4845=DIRECTION('',(0.,1.,0.));
#4846=DIRECTION('center_axis',(1.,0.,0.));
#4847=DIRECTION('ref_axis',(0.,0.,-1.));
#4848=DIRECTION('',(0.,-0.175790638483658,0.984427575508482));
#4849=DIRECTION('',(0.,-1.,0.));
#4850=DIRECTION('',(0.,1.,0.));
#4851=DIRECTION('',(0.,-1.,0.));
#4852=DIRECTION('',(0.,-1.,0.));
#4853=DIRECTION('',(0.,-1.,0.));
#4854=DIRECTION('center_axis',(0.,0.,-1.));
#4855=DIRECTION('ref_axis',(-1.,0.,0.));
#4856=DIRECTION('',(0.,1.,0.));
#4857=DIRECTION('',(-1.,0.,0.));
#4858=DIRECTION('',(0.,-1.,0.));
#4859=DIRECTION('',(-1.,1.50845519650157E-16,0.));
#4860=DIRECTION('',(0.,1.,0.));
#4861=DIRECTION('',(1.,-2.89120579329468E-16,0.));
#4862=DIRECTION('',(-1.,0.,0.));
#4863=DIRECTION('center_axis',(0.,0.,1.));
#4864=DIRECTION('ref_axis',(1.,0.,0.));
#4865=DIRECTION('',(0.,1.,0.));
#4866=DIRECTION('',(-1.,0.,0.));
#4867=DIRECTION('',(-1.,0.,0.));
#4868=DIRECTION('center_axis',(0.,0.,1.));
#4869=DIRECTION('ref_axis',(1.,0.,0.));
#4870=DIRECTION('',(0.,1.,0.));
#4871=DIRECTION('',(1.,0.,6.93889390390723E-16));
#4872=DIRECTION('',(0.,1.,0.));
#4873=DIRECTION('',(1.,0.,6.93889390390723E-16));
#4874=DIRECTION('',(1.,0.,6.93889390390723E-16));
#4875=DIRECTION('',(0.,-1.,0.));
#4876=DIRECTION('',(1.,0.,6.93889390390723E-16));
#4877=DIRECTION('',(-1.,0.,0.));
#4878=DIRECTION('',(0.,-1.,0.));
#4879=DIRECTION('',(-1.,0.,0.));
#4880=DIRECTION('center_axis',(0.,0.,-1.));
#4881=DIRECTION('ref_axis',(-1.,0.,0.));
#4882=DIRECTION('center_axis',(0.,0.,1.));
#4883=DIRECTION('ref_axis',(1.,0.,0.));
#4884=DIRECTION('',(0.,-1.,0.));
#4885=DIRECTION('center_axis',(0.,0.,-1.));
#4886=DIRECTION('ref_axis',(1.,1.22464679914735E-16,0.));
#4887=DIRECTION('',(0.,-0.175790638483658,-0.984427575508482));
#4888=DIRECTION('center_axis',(0.,0.,-1.));
#4889=DIRECTION('ref_axis',(-1.,0.,0.));
#4890=DIRECTION('',(0.,-1.,0.));
#4891=DIRECTION('center_axis',(0.,0.,-1.));
#4892=DIRECTION('ref_axis',(-1.,0.,0.));
#4893=DIRECTION('',(0.,-1.,0.));
#4894=DIRECTION('center_axis',(0.,0.,-1.));
#4895=DIRECTION('ref_axis',(-1.,0.,0.));
#4896=DIRECTION('',(0.,-1.,0.));
#4897=DIRECTION('center_axis',(1.,0.,0.));
#4898=DIRECTION('ref_axis',(0.,0.,-1.));
#4899=DIRECTION('',(0.,0.,-1.));
#4900=DIRECTION('',(0.,0.672272926960032,-0.740303391641961));
#4901=DIRECTION('center_axis',(1.,0.,0.));
#4902=DIRECTION('ref_axis',(0.,0.,-1.));
#4903=DIRECTION('',(0.,-0.669715115850366,-0.742618114242799));
#4904=DIRECTION('',(0.,0.,-1.));
#4905=DIRECTION('',(0.,0.,1.));
#4906=DIRECTION('',(0.,-0.669715115850366,0.742618114242799));
#4907=DIRECTION('center_axis',(1.,0.,0.));
#4908=DIRECTION('ref_axis',(0.,0.,1.));
#4909=DIRECTION('',(0.,0.672272926960032,0.740303391641961));
#4910=DIRECTION('',(0.,1.,0.));
#4911=DIRECTION('',(0.,0.,1.));
#4912=DIRECTION('',(0.,1.,0.));
#4913=DIRECTION('center_axis',(0.,1.,0.));
#4914=DIRECTION('ref_axis',(0.,0.,1.));
#4915=DIRECTION('',(-1.,0.,0.));
#4916=DIRECTION('center_axis',(0.,0.742618114242799,-0.669715115850366));
#4917=DIRECTION('ref_axis',(0.,0.669715115850366,0.742618114242799));
#4918=DIRECTION('',(-1.,0.,0.));
#4919=DIRECTION('center_axis',(-1.,0.,0.));
#4920=DIRECTION('ref_axis',(0.,0.,1.));
#4921=DIRECTION('',(-1.,0.,0.));
#4922=DIRECTION('center_axis',(0.,0.740303391641961,0.672272926960032));
#4923=DIRECTION('ref_axis',(0.,-0.672272926960032,0.740303391641961));
#4924=DIRECTION('center_axis',(0.,0.,1.));
#4925=DIRECTION('ref_axis',(1.,0.,0.));
#4926=DIRECTION('',(1.,-2.89120579329468E-16,0.));
#4927=DIRECTION('',(-1.,0.,0.));
#4928=DIRECTION('center_axis',(0.,-0.740303391641961,0.672272926960032));
#4929=DIRECTION('ref_axis',(0.,-0.672272926960032,-0.740303391641961));
#4930=DIRECTION('',(-1.,0.,0.));
#4931=DIRECTION('center_axis',(-1.,0.,0.));
#4932=DIRECTION('ref_axis',(0.,0.,1.));
#4933=DIRECTION('',(-1.,0.,0.));
#4934=DIRECTION('center_axis',(0.,-0.742618114242799,-0.669715115850366));
#4935=DIRECTION('ref_axis',(0.,0.669715115850366,-0.742618114242799));
#4936=DIRECTION('',(-1.,0.,0.));
#4937=DIRECTION('center_axis',(0.,-1.,0.));
#4938=DIRECTION('ref_axis',(0.,0.,-1.));
#4939=DIRECTION('center_axis',(-0.968938918897475,0.,0.247300164669968));
#4940=DIRECTION('ref_axis',(0.247300164669968,0.,0.968938918897475));
#4941=DIRECTION('',(-0.247300164669968,0.,-0.968938918897475));
#4942=DIRECTION('',(-0.247300164669968,0.,-0.968938918897475));
#4943=DIRECTION('center_axis',(0.,-1.,0.));
#4944=DIRECTION('ref_axis',(0.,0.,-1.));
#4945=DIRECTION('center_axis',(0.,-1.,0.));
#4946=DIRECTION('ref_axis',(0.,0.,-1.));
#4947=DIRECTION('center_axis',(0.968938918897475,0.,-0.247300164669968));
#4948=DIRECTION('ref_axis',(-0.247300164669968,0.,-0.968938918897475));
#4949=DIRECTION('',(-0.247300164669968,0.,-0.968938918897475));
#4950=DIRECTION('',(-0.247300164669968,0.,-0.968938918897475));
#4951=DIRECTION('center_axis',(0.,1.,0.));
#4952=DIRECTION('ref_axis',(0.,0.,-1.));
#4953=DIRECTION('center_axis',(0.,1.,0.));
#4954=DIRECTION('ref_axis',(0.,0.,-1.));
#4955=DIRECTION('center_axis',(0.,-1.,0.));
#4956=DIRECTION('ref_axis',(0.,0.,-1.));
#4957=DIRECTION('center_axis',(2.89120579329468E-16,1.,0.));
#4958=DIRECTION('ref_axis',(-1.,2.89120579329468E-16,0.));
#4959=DIRECTION('center_axis',(0.,0.,-1.));
#4960=DIRECTION('ref_axis',(-1.,0.,0.));
#4961=DIRECTION('',(1.,-1.50845519650157E-16,0.));
#4962=DIRECTION('',(0.,-1.,0.));
#4963=DIRECTION('',(0.,-1.,0.));
#4964=DIRECTION('',(-1.,0.,0.));
#4965=DIRECTION('center_axis',(0.,0.,-1.));
#4966=DIRECTION('ref_axis',(-1.,0.,0.));
#4967=DIRECTION('',(0.,-1.,0.));
#4968=DIRECTION('',(1.,-1.50845519650157E-16,0.));
#4969=DIRECTION('',(0.,-1.,0.));
#4970=DIRECTION('',(-1.,0.,0.));
#4971=DIRECTION('',(0.,-1.,0.));
#4972=DIRECTION('center_axis',(-1.,0.,0.));
#4973=DIRECTION('ref_axis',(0.,0.,1.));
#4974=DIRECTION('',(0.,0.,1.));
#4975=DIRECTION('',(0.,0.,1.));
#4976=DIRECTION('center_axis',(0.,1.,0.));
#4977=DIRECTION('ref_axis',(0.,0.,1.));
#4978=DIRECTION('',(0.,0.,-1.));
#4979=DIRECTION('center_axis',(-1.50845519650157E-16,-1.,0.));
#4980=DIRECTION('ref_axis',(1.,-1.50845519650157E-16,0.));
#4981=DIRECTION('',(0.,0.,1.));
#4982=DIRECTION('center_axis',(1.,0.,0.));
#4983=DIRECTION('ref_axis',(0.,0.,-1.));
#4984=DIRECTION('center_axis',(1.,0.,0.));
#4985=DIRECTION('ref_axis',(0.,0.,-1.));
#4986=DIRECTION('center_axis',(1.,0.,0.));
#4987=DIRECTION('ref_axis',(0.,0.,-1.));
#4988=DIRECTION('center_axis',(-1.,0.,0.));
#4989=DIRECTION('ref_axis',(0.,0.,1.));
#4990=DIRECTION('center_axis',(-1.,0.,0.));
#4991=DIRECTION('ref_axis',(0.,0.,1.));
#4992=DIRECTION('',(0.,0.,1.));
#4993=DIRECTION('',(1.,0.,0.));
#4994=DIRECTION('axis',(0.,0.,1.));
#4995=DIRECTION('refdir',(1.,0.,0.));
#4996=DIRECTION('center_axis',(0.,0.,1.));
#4997=DIRECTION('ref_axis',(1.,0.,0.));
#4998=DIRECTION('center_axis',(0.,0.,-1.));
#4999=DIRECTION('ref_axis',(-1.,0.,0.));
#5000=DIRECTION('',(0.,0.,-1.));
#5001=DIRECTION('center_axis',(0.,0.,1.));
#5002=DIRECTION('ref_axis',(1.,0.,0.));
#5003=DIRECTION('center_axis',(0.,0.,1.));
#5004=DIRECTION('ref_axis',(1.,0.,0.));
#5005=DIRECTION('center_axis',(0.,0.,1.));
#5006=DIRECTION('ref_axis',(1.,0.,0.));
#5007=DIRECTION('',(0.,0.,-1.));
#5008=DIRECTION('center_axis',(0.,0.,1.));
#5009=DIRECTION('ref_axis',(1.,0.,0.));
#5010=DIRECTION('center_axis',(0.,0.,1.));
#5011=DIRECTION('ref_axis',(1.,0.,0.));
#5012=DIRECTION('center_axis',(0.,0.,1.));
#5013=DIRECTION('ref_axis',(1.,0.,0.));
#5014=DIRECTION('',(0.,0.,-1.));
#5015=DIRECTION('center_axis',(0.,0.,-1.));
#5016=DIRECTION('ref_axis',(-1.,0.,0.));
#5017=DIRECTION('center_axis',(0.,0.,-1.));
#5018=DIRECTION('ref_axis',(-1.,0.,0.));
#5019=DIRECTION('center_axis',(0.,0.,-1.));
#5020=DIRECTION('ref_axis',(-1.,0.,0.));
#5021=DIRECTION('center_axis',(0.,0.,-1.));
#5022=DIRECTION('ref_axis',(-1.,0.,0.));
#5023=DIRECTION('center_axis',(0.,0.,1.));
#5024=DIRECTION('ref_axis',(1.,0.,0.));
#5025=DIRECTION('center_axis',(0.,0.,-1.));
#5026=DIRECTION('ref_axis',(-1.,0.,0.));
#5027=DIRECTION('center_axis',(0.,0.,-1.));
#5028=DIRECTION('ref_axis',(-1.,0.,0.));
#5029=DIRECTION('center_axis',(0.,0.,1.));
#5030=DIRECTION('ref_axis',(1.,0.,0.));
#5031=DIRECTION('center_axis',(0.,0.,1.));
#5032=DIRECTION('ref_axis',(1.,0.,0.));
#5033=DIRECTION('',(0.,0.,-1.));
#5034=DIRECTION('center_axis',(0.,0.,1.));
#5035=DIRECTION('ref_axis',(1.,0.,0.));
#5036=DIRECTION('center_axis',(0.,0.,-1.));
#5037=DIRECTION('ref_axis',(-1.,0.,0.));
#5038=DIRECTION('',(-0.5,0.866025403784438,0.));
#5039=DIRECTION('',(0.5,0.866025403784439,0.));
#5040=DIRECTION('',(1.,-1.25192883228096E-16,0.));
#5041=DIRECTION('',(0.5,-0.866025403784439,0.));
#5042=DIRECTION('',(-0.5,-0.866025403784439,0.));
#5043=DIRECTION('',(-1.,0.,0.));
#5044=DIRECTION('center_axis',(0.,0.,1.));
#5045=DIRECTION('ref_axis',(1.,0.,0.));
#5046=DIRECTION('center_axis',(0.866025403784439,-0.5,0.));
#5047=DIRECTION('ref_axis',(0.5,0.866025403784439,0.));
#5048=DIRECTION('',(0.,0.,1.));
#5049=DIRECTION('',(0.5,0.866025403784439,0.));
#5050=DIRECTION('',(0.,0.,1.));
#5051=DIRECTION('center_axis',(-1.25192883228096E-16,-1.,0.));
#5052=DIRECTION('ref_axis',(1.,-1.25192883228096E-16,0.));
#5053=DIRECTION('',(1.,-1.25192883228096E-16,0.));
#5054=DIRECTION('',(0.,0.,1.));
#5055=DIRECTION('center_axis',(-0.866025403784439,-0.5,0.));
#5056=DIRECTION('ref_axis',(0.5,-0.866025403784439,0.));
#5057=DIRECTION('',(0.5,-0.866025403784439,0.));
#5058=DIRECTION('',(0.,0.,1.));
#5059=DIRECTION('center_axis',(-0.866025403784439,0.5,0.));
#5060=DIRECTION('ref_axis',(-0.5,-0.866025403784439,0.));
#5061=DIRECTION('',(-0.5,-0.866025403784439,0.));
#5062=DIRECTION('',(0.,0.,1.));
#5063=DIRECTION('center_axis',(0.,1.,0.));
#5064=DIRECTION('ref_axis',(0.,0.,1.));
#5065=DIRECTION('',(-1.,0.,0.));
#5066=DIRECTION('',(0.,0.,1.));
#5067=DIRECTION('center_axis',(0.866025403784439,0.5,0.));
#5068=DIRECTION('ref_axis',(-0.5,0.866025403784439,0.));
#5069=DIRECTION('',(-0.5,0.866025403784438,0.));
#5070=DIRECTION('center_axis',(0.,0.,-1.));
#5071=DIRECTION('ref_axis',(-1.,0.,0.));
#5072=DIRECTION('center_axis',(0.,0.,-1.));
#5073=DIRECTION('ref_axis',(-1.,0.,0.));
#5074=DIRECTION('',(-0.995844981312748,-0.0910646649047396,0.));
#5075=DIRECTION('',(-0.576786803850996,0.816894719595709,0.));
#5076=DIRECTION('',(0.419058177461752,0.907959384500449,0.));
#5077=DIRECTION('',(0.995844981312748,0.0910646649047398,0.));
#5078=DIRECTION('',(0.576786803850996,-0.816894719595709,0.));
#5079=DIRECTION('',(-0.419058177461752,-0.907959384500449,0.));
#5080=DIRECTION('center_axis',(0.,0.,-1.));
#5081=DIRECTION('ref_axis',(-1.,0.,0.));
#5082=DIRECTION('',(0.419058177461752,0.907959384500449,0.));
#5083=DIRECTION('',(0.995844981312748,0.0910646649047398,0.));
#5084=DIRECTION('center_axis',(0.,0.,-1.));
#5085=DIRECTION('ref_axis',(-1.,0.,0.));
#5086=DIRECTION('',(0.995844981312748,0.0910646649047398,0.));
#5087=DIRECTION('',(0.576786803850996,-0.816894719595709,0.));
#5088=DIRECTION('center_axis',(0.,0.,-1.));
#5089=DIRECTION('ref_axis',(-1.,0.,0.));
#5090=DIRECTION('',(0.576786803850996,-0.816894719595709,0.));
#5091=DIRECTION('',(-0.419058177461752,-0.907959384500449,0.));
#5092=DIRECTION('center_axis',(0.,0.,-1.));
#5093=DIRECTION('ref_axis',(-1.,0.,0.));
#5094=DIRECTION('',(-0.419058177461752,-0.907959384500449,0.));
#5095=DIRECTION('',(-0.995844981312748,-0.0910646649047396,0.));
#5096=DIRECTION('center_axis',(0.,0.,-1.));
#5097=DIRECTION('ref_axis',(-1.,0.,0.));
#5098=DIRECTION('',(-0.995844981312748,-0.0910646649047396,0.));
#5099=DIRECTION('',(-0.576786803850996,0.816894719595709,0.));
#5100=DIRECTION('center_axis',(0.,0.,-1.));
#5101=DIRECTION('ref_axis',(-1.,0.,0.));
#5102=DIRECTION('',(-0.576786803850996,0.816894719595709,0.));
#5103=DIRECTION('',(0.419058177461752,0.907959384500449,0.));
#5104=DIRECTION('center_axis',(-0.0910646649047396,0.995844981312748,0.));
#5105=DIRECTION('ref_axis',(-0.995844981312748,-0.0910646649047396,0.));
#5106=DIRECTION('',(0.,0.,1.));
#5107=DIRECTION('',(0.,0.,1.));
#5108=DIRECTION('center_axis',(0.816894719595709,0.576786803850996,0.));
#5109=DIRECTION('ref_axis',(-0.576786803850996,0.816894719595709,0.));
#5110=DIRECTION('',(0.,0.,1.));
#5111=DIRECTION('center_axis',(0.907959384500449,-0.419058177461752,0.));
#5112=DIRECTION('ref_axis',(0.419058177461752,0.907959384500449,0.));
#5113=DIRECTION('',(0.,0.,1.));
#5114=DIRECTION('center_axis',(0.0910646649047398,-0.995844981312748,0.));
#5115=DIRECTION('ref_axis',(0.995844981312748,0.0910646649047399,0.));
#5116=DIRECTION('',(0.,0.,1.));
#5117=DIRECTION('center_axis',(-0.816894719595709,-0.576786803850996,0.));
#5118=DIRECTION('ref_axis',(0.576786803850996,-0.816894719595709,0.));
#5119=DIRECTION('',(0.,0.,1.));
#5120=DIRECTION('center_axis',(-0.907959384500449,0.419058177461752,0.));
#5121=DIRECTION('ref_axis',(-0.419058177461752,-0.907959384500449,0.));
#5122=DIRECTION('center_axis',(0.,0.,1.));
#5123=DIRECTION('ref_axis',(1.,0.,0.));
#5124=DIRECTION('center_axis',(0.,0.,1.));
#5125=DIRECTION('ref_axis',(1.,0.,0.));
#5126=DIRECTION('axis',(0.,0.,1.));
#5127=DIRECTION('refdir',(1.,0.,0.));
#5128=DIRECTION('center_axis',(-1.,0.,0.));
#5129=DIRECTION('ref_axis',(0.,0.,1.));
#5130=DIRECTION('center_axis',(-1.,0.,0.));
#5131=DIRECTION('ref_axis',(0.,0.,-1.));
#5132=DIRECTION('',(-1.,0.,0.));
#5133=DIRECTION('center_axis',(-1.,0.,0.));
#5134=DIRECTION('ref_axis',(0.,0.,-1.));
#5135=DIRECTION('',(-1.,0.,0.));
#5136=DIRECTION('center_axis',(-1.,0.,0.));
#5137=DIRECTION('ref_axis',(0.,0.,1.));
#5138=DIRECTION('center_axis',(1.,0.,0.));
#5139=DIRECTION('ref_axis',(0.,0.,-1.));
#5140=DIRECTION('',(-1.,0.,0.));
#5141=DIRECTION('center_axis',(1.,0.,0.));
#5142=DIRECTION('ref_axis',(0.,0.,-1.));
#5143=DIRECTION('',(-1.,0.,0.));
#5144=DIRECTION('center_axis',(-1.,0.,0.));
#5145=DIRECTION('ref_axis',(0.,0.,1.));
#5146=DIRECTION('center_axis',(1.,0.,0.));
#5147=DIRECTION('ref_axis',(0.,0.,-1.));
#5148=DIRECTION('',(-1.,0.,0.));
#5149=DIRECTION('center_axis',(1.,0.,0.));
#5150=DIRECTION('ref_axis',(0.,0.,-1.));
#5151=DIRECTION('',(-1.,0.,0.));
#5152=DIRECTION('center_axis',(0.,0.,-1.));
#5153=DIRECTION('ref_axis',(-1.,0.,0.));
#5154=DIRECTION('center_axis',(0.,0.,1.));
#5155=DIRECTION('ref_axis',(1.,0.,0.));
#5156=DIRECTION('',(0.,0.,-1.));
#5157=DIRECTION('center_axis',(0.,0.,1.));
#5158=DIRECTION('ref_axis',(1.,0.,0.));
#5159=DIRECTION('center_axis',(0.,0.,-1.));
#5160=DIRECTION('ref_axis',(-1.,0.,0.));
#5161=DIRECTION('center_axis',(0.,0.,1.));
#5162=DIRECTION('ref_axis',(1.,0.,0.));
#5163=DIRECTION('',(0.,0.,1.));
#5164=DIRECTION('center_axis',(0.,0.,1.));
#5165=DIRECTION('ref_axis',(1.,0.,0.));
#5166=DIRECTION('center_axis',(0.,0.,-1.));
#5167=DIRECTION('ref_axis',(-1.,0.,0.));
#5168=DIRECTION('center_axis',(0.,0.,1.));
#5169=DIRECTION('ref_axis',(1.,0.,0.));
#5170=DIRECTION('',(0.,0.,1.));
#5171=DIRECTION('center_axis',(0.,0.,-1.));
#5172=DIRECTION('ref_axis',(1.,0.,0.));
#5173=DIRECTION('center_axis',(0.,1.,0.));
#5174=DIRECTION('ref_axis',(1.,0.,0.));
#5175=DIRECTION('center_axis',(1.,0.,0.));
#5176=DIRECTION('ref_axis',(0.,0.,-1.));
#5177=DIRECTION('center_axis',(-1.,0.,0.));
#5178=DIRECTION('ref_axis',(0.,0.,1.));
#5179=DIRECTION('center_axis',(1.,-8.26058798084195E-17,0.));
#5180=DIRECTION('ref_axis',(-8.26058798084195E-17,-1.,0.));
#5181=DIRECTION('',(1.,0.,0.));
#5182=DIRECTION('center_axis',(-1.,0.,0.));
#5183=DIRECTION('ref_axis',(0.,0.,1.));
#5184=DIRECTION('center_axis',(1.,8.26058798084195E-17,0.));
#5185=DIRECTION('ref_axis',(8.26058798084195E-17,-1.,0.));
#5186=DIRECTION('',(1.,0.,0.));
#5187=DIRECTION('center_axis',(-1.,8.26058798084195E-17,0.));
#5188=DIRECTION('ref_axis',(8.26058798084195E-17,1.,0.));
#5189=DIRECTION('center_axis',(-1.,0.,0.));
#5190=DIRECTION('ref_axis',(0.,0.,1.));
#5191=DIRECTION('center_axis',(1.,0.,0.));
#5192=DIRECTION('ref_axis',(0.,0.,-1.));
#5193=DIRECTION('',(1.,0.,0.));
#5194=DIRECTION('center_axis',(-1.,-8.26058798084195E-17,0.));
#5195=DIRECTION('ref_axis',(8.26058798084195E-17,-1.,0.));
#5196=DIRECTION('center_axis',(0.,1.,-7.49879891330929E-33));
#5197=DIRECTION('ref_axis',(-1.,0.,-1.22464679914735E-16));
#5198=DIRECTION('center_axis',(-1.,0.,0.));
#5199=DIRECTION('ref_axis',(0.,0.,1.));
#5200=DIRECTION('center_axis',(1.,0.,0.));
#5201=DIRECTION('ref_axis',(0.,0.,-1.));
#5202=DIRECTION('',(1.,0.,0.));
#5203=DIRECTION('center_axis',(-1.,-8.26058798084195E-17,0.));
#5204=DIRECTION('ref_axis',(8.26058798084195E-17,-1.,0.));
#5205=DIRECTION('center_axis',(-1.,0.,0.));
#5206=DIRECTION('ref_axis',(0.,0.,1.));
#5207=DIRECTION('center_axis',(1.,-8.26058798084195E-17,0.));
#5208=DIRECTION('ref_axis',(-8.26058798084195E-17,-1.,0.));
#5209=DIRECTION('',(1.,0.,0.));
#5210=DIRECTION('center_axis',(-1.,-8.26058798084195E-17,0.));
#5211=DIRECTION('ref_axis',(-8.26058798084195E-17,1.,0.));
#5212=DIRECTION('center_axis',(-1.,0.,0.));
#5213=DIRECTION('ref_axis',(0.,0.,1.));
#5214=DIRECTION('center_axis',(1.,8.26058798084195E-17,0.));
#5215=DIRECTION('ref_axis',(8.26058798084195E-17,-1.,0.));
#5216=DIRECTION('',(1.,0.,0.));
#5217=DIRECTION('center_axis',(1.,0.,0.));
#5218=DIRECTION('ref_axis',(0.,0.,-1.));
#5219=DIRECTION('center_axis',(1.,0.,0.));
#5220=DIRECTION('ref_axis',(0.,0.,-1.));
#5221=DIRECTION('center_axis',(1.,0.,0.));
#5222=DIRECTION('ref_axis',(0.,0.,-1.));
#5223=DIRECTION('',(-1.,0.,0.));
#5224=DIRECTION('center_axis',(1.,0.,0.));
#5225=DIRECTION('ref_axis',(0.,0.,-1.));
#5226=DIRECTION('',(1.,0.,0.));
#5227=DIRECTION('center_axis',(0.,0.,1.));
#5228=DIRECTION('ref_axis',(1.,0.,0.));
#5229=DIRECTION('',(8.26058798084195E-17,1.,0.));
#5230=DIRECTION('',(-1.,0.,0.));
#5231=DIRECTION('',(-8.26058798084195E-17,-1.,0.));
#5232=DIRECTION('',(-1.,0.,0.));
#5233=DIRECTION('',(-8.26058798084195E-17,1.,0.));
#5234=DIRECTION('',(-1.,0.,0.));
#5235=DIRECTION('',(8.26058798084195E-17,-1.,0.));
#5236=DIRECTION('',(-1.,-3.85494105772624E-15,0.));
#5237=DIRECTION('',(0.,-1.,0.));
#5238=DIRECTION('',(1.,-3.85494105772624E-15,0.));
#5239=DIRECTION('',(-8.26058798084195E-17,-1.,0.));
#5240=DIRECTION('',(-1.,0.,0.));
#5241=DIRECTION('',(8.26058798084195E-17,1.,0.));
#5242=DIRECTION('',(1.,0.,0.));
#5243=DIRECTION('',(8.26058798084195E-17,-1.,0.));
#5244=DIRECTION('',(-1.,0.,0.));
#5245=DIRECTION('',(-8.26058798084195E-17,1.,0.));
#5246=DIRECTION('',(1.,3.85494105772624E-15,0.));
#5247=DIRECTION('',(0.,1.,0.));
#5248=DIRECTION('',(-1.,3.85494105772624E-15,0.));
#5249=DIRECTION('center_axis',(0.,0.,1.));
#5250=DIRECTION('ref_axis',(1.,0.,0.));
#5251=DIRECTION('',(-1.,0.,0.));
#5252=DIRECTION('',(8.26058798084195E-17,1.,0.));
#5253=DIRECTION('',(-1.,3.85494105772624E-15,0.));
#5254=DIRECTION('',(0.,1.,0.));
#5255=DIRECTION('',(1.,3.85494105772624E-15,0.));
#5256=DIRECTION('',(-8.26058798084195E-17,1.,0.));
#5257=DIRECTION('',(-1.,0.,0.));
#5258=DIRECTION('',(8.26058798084195E-17,-1.,0.));
#5259=DIRECTION('',(1.,0.,0.));
#5260=DIRECTION('',(8.26058798084195E-17,1.,0.));
#5261=DIRECTION('',(-1.,0.,0.));
#5262=DIRECTION('',(-8.26058798084195E-17,-1.,0.));
#5263=DIRECTION('',(1.,-3.85494105772624E-15,0.));
#5264=DIRECTION('',(0.,-1.,0.));
#5265=DIRECTION('',(-1.,-3.85494105772624E-15,0.));
#5266=DIRECTION('',(8.26058798084195E-17,-1.,0.));
#5267=DIRECTION('',(-1.,0.,0.));
#5268=DIRECTION('',(-8.26058798084195E-17,1.,0.));
#5269=DIRECTION('',(-1.,0.,0.));
#5270=DIRECTION('',(-8.26058798084195E-17,-1.,0.));
#5271=DIRECTION('center_axis',(1.,-8.26058798084195E-17,0.));
#5272=DIRECTION('ref_axis',(8.26058798084195E-17,1.,0.));
#5273=DIRECTION('center_axis',(1.,-8.26058798084195E-17,0.));
#5274=DIRECTION('ref_axis',(8.26058798084195E-17,1.,0.));
#5275=DIRECTION('',(0.,0.,-1.));
#5276=DIRECTION('center_axis',(-1.,8.26058798084195E-17,0.));
#5277=DIRECTION('ref_axis',(-8.26058798084195E-17,-1.,0.));
#5278=DIRECTION('center_axis',(-1.,8.26058798084195E-17,0.));
#5279=DIRECTION('ref_axis',(-8.26058798084195E-17,-1.,0.));
#5280=DIRECTION('',(0.,0.,-1.));
#5281=DIRECTION('center_axis',(1.,8.26058798084195E-17,0.));
#5282=DIRECTION('ref_axis',(-8.26058798084195E-17,1.,0.));
#5283=DIRECTION('center_axis',(1.,8.26058798084195E-17,0.));
#5284=DIRECTION('ref_axis',(-8.26058798084195E-17,1.,0.));
#5285=DIRECTION('',(0.,0.,-1.));
#5286=DIRECTION('center_axis',(-1.,-8.26058798084195E-17,0.));
#5287=DIRECTION('ref_axis',(8.26058798084195E-17,-1.,0.));
#5288=DIRECTION('center_axis',(-1.,-8.26058798084195E-17,0.));
#5289=DIRECTION('ref_axis',(8.26058798084195E-17,-1.,0.));
#5290=DIRECTION('',(0.,0.,-1.));
#5291=DIRECTION('center_axis',(-1.,8.26058798084195E-17,0.));
#5292=DIRECTION('ref_axis',(-8.26058798084195E-17,-1.,0.));
#5293=DIRECTION('center_axis',(-1.,8.26058798084195E-17,0.));
#5294=DIRECTION('ref_axis',(-8.26058798084195E-17,-1.,0.));
#5295=DIRECTION('',(0.,0.,-1.));
#5296=DIRECTION('center_axis',(1.,-8.26058798084195E-17,0.));
#5297=DIRECTION('ref_axis',(8.26058798084195E-17,1.,0.));
#5298=DIRECTION('center_axis',(1.,-8.26058798084195E-17,0.));
#5299=DIRECTION('ref_axis',(8.26058798084195E-17,1.,0.));
#5300=DIRECTION('',(0.,0.,-1.));
#5301=DIRECTION('center_axis',(-1.,-8.26058798084195E-17,0.));
#5302=DIRECTION('ref_axis',(8.26058798084195E-17,-1.,0.));
#5303=DIRECTION('center_axis',(-1.,-8.26058798084195E-17,0.));
#5304=DIRECTION('ref_axis',(8.26058798084195E-17,-1.,0.));
#5305=DIRECTION('',(0.,0.,-1.));
#5306=DIRECTION('center_axis',(1.,8.26058798084195E-17,0.));
#5307=DIRECTION('ref_axis',(-8.26058798084195E-17,1.,0.));
#5308=DIRECTION('center_axis',(1.,8.26058798084195E-17,0.));
#5309=DIRECTION('ref_axis',(-8.26058798084195E-17,1.,0.));
#5310=DIRECTION('',(0.,0.,-1.));
#5311=DIRECTION('center_axis',(3.85494105772624E-15,-1.,0.));
#5312=DIRECTION('ref_axis',(1.,3.85494105772624E-15,0.));
#5313=DIRECTION('',(0.,0.,-1.));
#5314=DIRECTION('center_axis',(1.,0.,0.));
#5315=DIRECTION('ref_axis',(0.,0.,-1.));
#5316=DIRECTION('',(0.,0.,-1.));
#5317=DIRECTION('center_axis',(3.85494105772624E-15,1.,0.));
#5318=DIRECTION('ref_axis',(-1.,3.85494105772624E-15,0.));
#5319=DIRECTION('center_axis',(0.,1.,0.));
#5320=DIRECTION('ref_axis',(0.,0.,1.));
#5321=DIRECTION('center_axis',(-3.85494105772624E-15,1.,0.));
#5322=DIRECTION('ref_axis',(-1.,-3.85494105772624E-15,0.));
#5323=DIRECTION('',(0.,0.,-1.));
#5324=DIRECTION('center_axis',(-1.,0.,0.));
#5325=DIRECTION('ref_axis',(0.,0.,1.));
#5326=DIRECTION('',(0.,0.,-1.));
#5327=DIRECTION('center_axis',(-3.85494105772624E-15,-1.,0.));
#5328=DIRECTION('ref_axis',(1.,-3.85494105772624E-15,0.));
#5329=DIRECTION('center_axis',(0.,-1.,0.));
#5330=DIRECTION('ref_axis',(0.,0.,-1.));
#5331=DIRECTION('center_axis',(-1.,0.,0.));
#5332=DIRECTION('ref_axis',(0.,0.,1.));
#5333=DIRECTION('center_axis',(-1.,0.,0.));
#5334=DIRECTION('ref_axis',(0.,0.,1.));
#5335=DIRECTION('center_axis',(-1.,0.,0.));
#5336=DIRECTION('ref_axis',(0.,0.,1.));
#5337=DIRECTION('center_axis',(-1.,0.,0.));
#5338=DIRECTION('ref_axis',(0.,0.,1.));
#5339=DIRECTION('center_axis',(1.,0.,0.));
#5340=DIRECTION('ref_axis',(0.,0.,-1.));
#5341=DIRECTION('center_axis',(1.,0.,0.));
#5342=DIRECTION('ref_axis',(0.,0.,-1.));
#5343=DIRECTION('center_axis',(0.,0.,1.));
#5344=DIRECTION('ref_axis',(1.,0.,0.));
#5345=DIRECTION('center_axis',(0.,0.,1.));
#5346=DIRECTION('ref_axis',(1.,0.,0.));
#5347=DIRECTION('center_axis',(0.,1.,0.));
#5348=DIRECTION('ref_axis',(0.,0.,1.));
#5349=DIRECTION('',(0.,0.,-1.));
#5350=DIRECTION('',(0.,0.,-1.));
#5351=DIRECTION('center_axis',(0.,-1.,0.));
#5352=DIRECTION('ref_axis',(0.,0.,-1.));
#5353=DIRECTION('',(0.,0.,1.));
#5354=DIRECTION('',(0.,0.,1.));
#5355=DIRECTION('center_axis',(1.,0.,0.));
#5356=DIRECTION('ref_axis',(0.,0.,-1.));
#5357=DIRECTION('center_axis',(1.,0.,0.));
#5358=DIRECTION('ref_axis',(0.,0.,-1.));
#5359=DIRECTION('axis',(0.,0.,1.));
#5360=DIRECTION('refdir',(1.,0.,0.));
#5361=DIRECTION('center_axis',(0.,0.,-1.));
#5362=DIRECTION('ref_axis',(-1.,0.,0.));
#5363=DIRECTION('center_axis',(0.,0.,1.));
#5364=DIRECTION('ref_axis',(1.,0.,0.));
#5365=DIRECTION('',(0.,0.,-1.));
#5366=DIRECTION('center_axis',(0.,0.,1.));
#5367=DIRECTION('ref_axis',(1.,0.,0.));
#5368=DIRECTION('center_axis',(0.,0.,-1.));
#5369=DIRECTION('ref_axis',(-1.,0.,0.));
#5370=DIRECTION('center_axis',(0.,0.,1.));
#5371=DIRECTION('ref_axis',(1.,0.,0.));
#5372=DIRECTION('',(0.,0.,-1.));
#5373=DIRECTION('center_axis',(0.,0.,1.));
#5374=DIRECTION('ref_axis',(1.,0.,0.));
#5375=DIRECTION('center_axis',(0.,0.,-1.));
#5376=DIRECTION('ref_axis',(-1.,0.,0.));
#5377=DIRECTION('center_axis',(0.,0.,1.));
#5378=DIRECTION('ref_axis',(1.,0.,0.));
#5379=DIRECTION('',(0.,0.,-1.));
#5380=DIRECTION('center_axis',(0.,0.,1.));
#5381=DIRECTION('ref_axis',(1.,0.,0.));
#5382=DIRECTION('',(0.,0.,-1.));
#5383=DIRECTION('center_axis',(0.,0.,1.));
#5384=DIRECTION('ref_axis',(1.,0.,0.));
#5385=DIRECTION('',(1.,1.44560289664734E-16,0.));
#5386=DIRECTION('center_axis',(0.,0.,1.));
#5387=DIRECTION('ref_axis',(-1.,0.,0.));
#5388=DIRECTION('',(-1.,0.,0.));
#5389=DIRECTION('center_axis',(0.,0.,1.));
#5390=DIRECTION('ref_axis',(1.,0.,0.));
#5391=DIRECTION('',(-1.,0.,0.));
#5392=DIRECTION('center_axis',(0.,0.,1.));
#5393=DIRECTION('ref_axis',(-1.,0.,0.));
#5394=DIRECTION('',(1.,1.44560289664734E-16,0.));
#5395=DIRECTION('center_axis',(-1.44560289664734E-16,1.,0.));
#5396=DIRECTION('ref_axis',(-1.,-1.44560289664734E-16,0.));
#5397=DIRECTION('',(0.,0.,-1.));
#5398=DIRECTION('center_axis',(0.,0.,-1.));
#5399=DIRECTION('ref_axis',(1.,1.22464679914735E-16,0.));
#5400=DIRECTION('',(0.,0.,-1.));
#5401=DIRECTION('center_axis',(0.,-1.,0.));
#5402=DIRECTION('ref_axis',(0.,0.,-1.));
#5403=DIRECTION('axis',(0.,0.,1.));
#5404=DIRECTION('refdir',(1.,0.,0.));
#5405=DIRECTION('center_axis',(0.,0.,-1.));
#5406=DIRECTION('ref_axis',(-1.,0.,0.));
#5407=DIRECTION('center_axis',(0.,0.,-1.));
#5408=DIRECTION('ref_axis',(1.,0.,0.));
#5409=DIRECTION('',(-0.707106781186551,8.65956056235497E-17,0.707106781186544));
#5410=DIRECTION('center_axis',(0.,0.,1.));
#5411=DIRECTION('ref_axis',(1.,0.,0.));
#5412=DIRECTION('center_axis',(0.,0.,-1.));
#5413=DIRECTION('ref_axis',(-1.,0.,0.));
#5414=DIRECTION('center_axis',(0.,0.,-1.));
#5415=DIRECTION('ref_axis',(1.,0.,0.));
#5416=DIRECTION('',(-0.707106781186551,8.65956056235498E-17,0.707106781186544));
#5417=DIRECTION('center_axis',(0.,0.,1.));
#5418=DIRECTION('ref_axis',(1.,0.,0.));
#5419=DIRECTION('center_axis',(0.,0.,1.));
#5420=DIRECTION('ref_axis',(1.,0.,0.));
#5421=DIRECTION('center_axis',(0.,0.,1.));
#5422=DIRECTION('ref_axis',(1.,0.,0.));
#5423=DIRECTION('center_axis',(0.,0.,1.));
#5424=DIRECTION('ref_axis',(1.,0.,0.));
#5425=DIRECTION('',(0.707106781186543,8.65956056235488E-17,-0.707106781186551));
#5426=DIRECTION('center_axis',(0.,0.,-1.));
#5427=DIRECTION('ref_axis',(1.,0.,0.));
#5428=DIRECTION('center_axis',(0.,0.,1.));
#5429=DIRECTION('ref_axis',(1.,0.,0.));
#5430=DIRECTION('center_axis',(0.,0.,1.));
#5431=DIRECTION('ref_axis',(1.,0.,0.));
#5432=DIRECTION('center_axis',(0.,0.,1.));
#5433=DIRECTION('ref_axis',(1.,0.,0.));
#5434=DIRECTION('',(0.707106781186543,8.65956056235488E-17,-0.707106781186551));
#5435=DIRECTION('center_axis',(0.,0.,-1.));
#5436=DIRECTION('ref_axis',(1.,0.,0.));
#5437=DIRECTION('center_axis',(0.,0.,-1.));
#5438=DIRECTION('ref_axis',(-1.,0.,0.));
#5439=DIRECTION('center_axis',(0.,0.,1.));
#5440=DIRECTION('ref_axis',(1.,0.,0.));
#5441=DIRECTION('',(0.,0.,1.));
#5442=DIRECTION('center_axis',(0.,0.,-1.));
#5443=DIRECTION('ref_axis',(-1.,0.,0.));
#5444=DIRECTION('',(0.,0.,1.));
#5445=DIRECTION('center_axis',(0.,0.,1.));
#5446=DIRECTION('ref_axis',(-1.,0.,0.));
#5447=DIRECTION('center_axis',(0.,0.,-1.));
#5448=DIRECTION('ref_axis',(-1.,0.,0.));
#5449=DIRECTION('center_axis',(0.,0.,1.));
#5450=DIRECTION('ref_axis',(1.,0.,0.));
#5451=DIRECTION('',(0.,0.,1.));
#5452=DIRECTION('center_axis',(0.,0.,-1.));
#5453=DIRECTION('ref_axis',(1.,0.,0.));
#5454=DIRECTION('center_axis',(0.,0.,-1.));
#5455=DIRECTION('ref_axis',(-1.,0.,0.));
#5456=DIRECTION('center_axis',(0.,0.,1.));
#5457=DIRECTION('ref_axis',(1.,0.,0.));
#5458=DIRECTION('',(0.,0.,1.));
#5459=DIRECTION('center_axis',(0.,0.,-1.));
#5460=DIRECTION('ref_axis',(-1.,0.,0.));
#5461=DIRECTION('',(0.,0.,1.));
#5462=DIRECTION('center_axis',(0.,0.,1.));
#5463=DIRECTION('ref_axis',(-1.,0.,0.));
#5464=DIRECTION('center_axis',(0.,0.,-1.));
#5465=DIRECTION('ref_axis',(-1.,0.,0.));
#5466=DIRECTION('center_axis',(0.,0.,1.));
#5467=DIRECTION('ref_axis',(-1.,0.,0.));
#5468=DIRECTION('center_axis',(0.258819045102526,0.965925826289067,0.));
#5469=DIRECTION('ref_axis',(-0.965925826289067,0.258819045102526,0.));
#5470=DIRECTION('center_axis',(0.,0.,-1.));
#5471=DIRECTION('ref_axis',(-1.,0.,0.));
#5472=DIRECTION('center_axis',(-0.258819045102523,-0.965925826289068,0.));
#5473=DIRECTION('ref_axis',(0.965925826289068,-0.258819045102523,0.));
#5474=DIRECTION('center_axis',(0.,0.,1.));
#5475=DIRECTION('ref_axis',(1.,0.,0.));
#5476=DIRECTION('center_axis',(0.,0.,1.));
#5477=DIRECTION('ref_axis',(1.,0.,0.));
#5478=DIRECTION('center_axis',(0.547412572866653,-0.836862877099655,0.));
#5479=DIRECTION('ref_axis',(0.836862877099655,0.547412572866653,0.));
#5480=DIRECTION('center_axis',(0.,0.,-1.));
#5481=DIRECTION('ref_axis',(1.,-2.66453525910038E-15,0.));
#5482=DIRECTION('center_axis',(-0.666666666666666,0.74535599249993,0.));
#5483=DIRECTION('ref_axis',(-0.74535599249993,-0.666666666666666,0.));
#5484=DIRECTION('center_axis',(0.,0.,1.));
#5485=DIRECTION('ref_axis',(1.,0.,0.));
#5486=DIRECTION('center_axis',(0.,0.,1.));
#5487=DIRECTION('ref_axis',(1.,0.,0.));
#5488=DIRECTION('center_axis',(0.,0.,-1.));
#5489=DIRECTION('ref_axis',(1.,0.,0.));
#5490=DIRECTION('center_axis',(-1.,0.,0.));
#5491=DIRECTION('ref_axis',(0.,0.,1.));
#5492=DIRECTION('center_axis',(0.,0.,1.));
#5493=DIRECTION('ref_axis',(1.,0.,0.));
#5494=DIRECTION('center_axis',(-1.,0.,0.));
#5495=DIRECTION('ref_axis',(0.,0.,1.));
#5496=DIRECTION('center_axis',(0.,0.,1.));
#5497=DIRECTION('ref_axis',(-1.,0.,0.));
#5498=DIRECTION('center_axis',(0.,0.,1.));
#5499=DIRECTION('ref_axis',(1.,0.,0.));
#5500=DIRECTION('',(0.,0.,1.));
#5501=DIRECTION('center_axis',(0.,0.,1.));
#5502=DIRECTION('ref_axis',(1.,0.,0.));
#5503=DIRECTION('center_axis',(0.,0.,1.));
#5504=DIRECTION('ref_axis',(-1.,0.,0.));
#5505=DIRECTION('',(0.,0.,1.));
#5506=DIRECTION('center_axis',(0.,0.,1.));
#5507=DIRECTION('ref_axis',(1.,0.,0.));
#5508=DIRECTION('',(0.,0.,1.));
#5509=DIRECTION('center_axis',(0.,0.,-1.));
#5510=DIRECTION('ref_axis',(-1.,0.,0.));
#5511=DIRECTION('center_axis',(0.,0.,1.));
#5512=DIRECTION('ref_axis',(1.,0.,0.));
#5513=DIRECTION('',(0.,0.,-1.));
#5514=DIRECTION('center_axis',(0.,0.,1.));
#5515=DIRECTION('ref_axis',(1.,0.,0.));
#5516=DIRECTION('center_axis',(0.,0.,-1.));
#5517=DIRECTION('ref_axis',(-1.,0.,0.));
#5518=DIRECTION('center_axis',(0.,0.,-1.));
#5519=DIRECTION('ref_axis',(1.,0.,0.));
#5520=DIRECTION('',(0.,0.,-1.));
#5521=DIRECTION('center_axis',(0.,0.,1.));
#5522=DIRECTION('ref_axis',(1.,0.,0.));
#5523=DIRECTION('',(0.,0.,-1.));
#5524=DIRECTION('center_axis',(0.,0.,-1.));
#5525=DIRECTION('ref_axis',(-1.,0.,0.));
#5526=DIRECTION('center_axis',(0.,0.,1.));
#5527=DIRECTION('ref_axis',(1.,0.,0.));
#5528=DIRECTION('',(0.,0.,1.));
#5529=DIRECTION('center_axis',(0.,0.,-1.));
#5530=DIRECTION('ref_axis',(-1.,0.,0.));
#5531=DIRECTION('',(0.,0.,-1.));
#5532=DIRECTION('',(0.,0.,1.));
#5533=DIRECTION('center_axis',(0.,0.,1.));
#5534=DIRECTION('ref_axis',(1.,0.,0.));
#5535=DIRECTION('',(0.,0.,-1.));
#5536=DIRECTION('center_axis',(0.,0.,-1.));
#5537=DIRECTION('ref_axis',(-1.,0.,0.));
#5538=DIRECTION('center_axis',(0.,0.,1.));
#5539=DIRECTION('ref_axis',(1.,0.,0.));
#5540=DIRECTION('',(-0.258819045102525,-0.965925826289067,0.));
#5541=DIRECTION('center_axis',(0.,0.,1.));
#5542=DIRECTION('ref_axis',(1.,0.,0.));
#5543=DIRECTION('',(0.258819045102524,0.965925826289067,0.));
#5544=DIRECTION('center_axis',(0.,0.,-1.));
#5545=DIRECTION('ref_axis',(1.,0.,0.));
#5546=DIRECTION('',(1.,-6.088865147686E-17,0.));
#5547=DIRECTION('',(-3.46944695195361E-16,1.,0.));
#5548=DIRECTION('',(-1.,0.,0.));
#5549=DIRECTION('center_axis',(0.965925826289067,-0.258819045102525,0.));
#5550=DIRECTION('ref_axis',(0.258819045102525,0.965925826289067,0.));
#5551=DIRECTION('',(0.258819045102525,0.965925826289067,0.));
#5552=DIRECTION('',(-0.258819045102525,-0.965925826289067,0.));
#5553=DIRECTION('',(-0.258819045102525,-0.965925826289067,0.));
#5554=DIRECTION('',(0.,0.,-1.));
#5555=DIRECTION('',(-0.258819045102525,-0.965925826289067,0.));
#5556=DIRECTION('center_axis',(-0.965925826289067,0.258819045102524,0.));
#5557=DIRECTION('ref_axis',(-0.258819045102524,-0.965925826289067,0.));
#5558=DIRECTION('',(0.,0.,-1.));
#5559=DIRECTION('',(-0.258819045102524,-0.965925826289067,0.));
#5560=DIRECTION('',(0.258819045102524,0.965925826289067,0.));
#5561=DIRECTION('',(0.,0.,-1.));
#5562=DIRECTION('',(0.258819045102524,0.965925826289067,0.));
#5563=DIRECTION('',(0.258819045102524,0.965925826289067,0.));
#5564=DIRECTION('center_axis',(0.,0.,-1.));
#5565=DIRECTION('ref_axis',(-1.,0.,0.));
#5566=DIRECTION('',(0.,0.,-1.));
#5567=DIRECTION('center_axis',(0.,0.,1.));
#5568=DIRECTION('ref_axis',(1.,0.,0.));
#5569=DIRECTION('center_axis',(0.,0.,-1.));
#5570=DIRECTION('ref_axis',(-1.,0.,0.));
#5571=DIRECTION('center_axis',(6.088865147686E-17,1.,0.));
#5572=DIRECTION('ref_axis',(-1.,6.088865147686E-17,0.));
#5573=DIRECTION('',(0.,0.,-1.));
#5574=DIRECTION('',(-1.,6.088865147686E-17,0.));
#5575=DIRECTION('center_axis',(-6.088865147686E-17,-1.,0.));
#5576=DIRECTION('ref_axis',(-1.,6.088865147686E-17,0.));
#5577=DIRECTION('',(0.,0.,-1.));
#5578=DIRECTION('center_axis',(-6.088865147686E-17,-1.,0.));
#5579=DIRECTION('ref_axis',(-1.,6.088865147686E-17,0.));
#5580=DIRECTION('',(-1.,6.088865147686E-17,0.));
#5581=DIRECTION('',(1.,-6.088865147686E-17,0.));
#5582=DIRECTION('center_axis',(-6.088865147686E-17,-1.,0.));
#5583=DIRECTION('ref_axis',(-1.,6.088865147686E-17,0.));
#5584=DIRECTION('',(0.,0.,-1.));
#5585=DIRECTION('center_axis',(-6.088865147686E-17,-1.,0.));
#5586=DIRECTION('ref_axis',(-1.,6.088865147686E-17,0.));
#5587=DIRECTION('',(1.,-6.088865147686E-17,0.));
#5588=DIRECTION('',(0.,0.,1.));
#5589=DIRECTION('',(1.,-6.67201336914156E-17,0.));
#5590=DIRECTION('',(0.,0.,-1.));
#5591=DIRECTION('',(1.,-6.67201336914156E-17,0.));
#5592=DIRECTION('center_axis',(0.,-1.,0.));
#5593=DIRECTION('ref_axis',(0.,0.,-1.));
#5594=DIRECTION('center_axis',(0.,1.,0.));
#5595=DIRECTION('ref_axis',(0.,0.,-1.));
#5596=DIRECTION('',(1.,0.,0.));
#5597=DIRECTION('',(0.,0.,-1.));
#5598=DIRECTION('',(-1.,0.,0.));
#5599=DIRECTION('',(0.,0.,-1.));
#5600=DIRECTION('',(-1.,0.,0.));
#5601=DIRECTION('',(0.,0.,1.));
#5602=DIRECTION('',(-1.,0.,0.));
#5603=DIRECTION('center_axis',(0.,1.,0.));
#5604=DIRECTION('ref_axis',(0.,0.,-1.));
#5605=DIRECTION('',(0.,0.,1.));
#5606=DIRECTION('center_axis',(0.,1.,0.));
#5607=DIRECTION('ref_axis',(0.,0.,-1.));
#5608=DIRECTION('',(-1.,0.,0.));
#5609=DIRECTION('',(1.,0.,0.));
#5610=DIRECTION('center_axis',(0.,1.,0.));
#5611=DIRECTION('ref_axis',(0.,0.,-1.));
#5612=DIRECTION('',(0.,0.,1.));
#5613=DIRECTION('center_axis',(0.,0.,1.));
#5614=DIRECTION('ref_axis',(1.,0.,0.));
#5615=DIRECTION('',(3.46944695195361E-16,-1.,0.));
#5616=DIRECTION('',(1.,-6.088865147686E-17,0.));
#5617=DIRECTION('',(-1.,0.,0.));
#5618=DIRECTION('center_axis',(0.,0.,-1.));
#5619=DIRECTION('ref_axis',(1.,1.22464679914735E-16,0.));
#5620=DIRECTION('center_axis',(0.,0.,1.));
#5621=DIRECTION('ref_axis',(1.,0.,0.));
#5622=DIRECTION('center_axis',(1.,-3.46944695195361E-16,0.));
#5623=DIRECTION('ref_axis',(3.46944695195361E-16,1.,0.));
#5624=DIRECTION('',(-3.46944695195361E-16,-1.,0.));
#5625=DIRECTION('',(-3.46944695195361E-16,-1.,0.));
#5626=DIRECTION('center_axis',(0.,0.,1.));
#5627=DIRECTION('ref_axis',(1.,0.,0.));
#5628=DIRECTION('center_axis',(-0.258819045102524,-0.965925826289067,0.));
#5629=DIRECTION('ref_axis',(0.965925826289067,-0.258819045102524,0.));
#5630=DIRECTION('',(-0.965925826289067,0.258819045102524,0.));
#5631=DIRECTION('',(-0.965925826289067,0.258819045102524,0.));
#5632=DIRECTION('center_axis',(0.,0.,1.));
#5633=DIRECTION('ref_axis',(1.,0.,0.));
#5634=DIRECTION('center_axis',(1.,3.46944695195361E-16,0.));
#5635=DIRECTION('ref_axis',(-3.46944695195361E-16,1.,0.));
#5636=DIRECTION('',(-3.46944695195361E-16,1.,0.));
#5637=DIRECTION('',(0.,0.,-1.));
#5638=DIRECTION('',(3.46944695195361E-16,-1.,0.));
#5639=DIRECTION('',(0.,0.,1.));
#5640=DIRECTION('center_axis',(0.,0.,1.));
#5641=DIRECTION('ref_axis',(1.,0.,0.));
#5642=DIRECTION('center_axis',(0.,0.,-1.));
#5643=DIRECTION('ref_axis',(1.,0.,0.));
#5644=DIRECTION('',(-0.258819045102524,-0.965925826289067,0.));
#5645=DIRECTION('',(0.258819045102525,0.965925826289067,0.));
#5646=DIRECTION('center_axis',(0.,0.,1.));
#5647=DIRECTION('ref_axis',(-1.,0.,0.));
#5648=DIRECTION('',(1.,0.,0.));
#5649=DIRECTION('',(3.46944695195361E-16,-1.,0.));
#5650=DIRECTION('',(-1.,6.088865147686E-17,0.));
#5651=DIRECTION('center_axis',(0.,0.,1.));
#5652=DIRECTION('ref_axis',(-1.,9.46212805078258E-16,0.));
#5653=DIRECTION('center_axis',(0.,0.,-1.));
#5654=DIRECTION('ref_axis',(1.,0.,0.));
#5655=DIRECTION('center_axis',(0.,0.,-1.));
#5656=DIRECTION('ref_axis',(-1.,0.,0.));
#5657=DIRECTION('',(-1.,6.088865147686E-17,0.));
#5658=DIRECTION('',(-3.46944695195361E-16,1.,0.));
#5659=DIRECTION('',(1.,0.,0.));
#5660=DIRECTION('center_axis',(0.,0.,1.));
#5661=DIRECTION('ref_axis',(1.,-1.22464679914735E-16,0.));
#5662=DIRECTION('center_axis',(0.,0.,1.));
#5663=DIRECTION('ref_axis',(-1.,0.,0.));
#5664=DIRECTION('center_axis',(0.,0.,1.));
#5665=DIRECTION('ref_axis',(1.,0.,0.));
#5666=DIRECTION('center_axis',(0.,0.,-1.));
#5667=DIRECTION('ref_axis',(1.,0.,0.));
#5668=DIRECTION('center_axis',(0.,0.,-1.));
#5669=DIRECTION('ref_axis',(1.,0.,0.));
#5670=DIRECTION('center_axis',(1.,3.46944695195361E-16,0.));
#5671=DIRECTION('ref_axis',(-3.46944695195361E-16,1.,0.));
#5672=DIRECTION('',(3.46944695195361E-16,-1.,0.));
#5673=DIRECTION('',(0.,0.,1.));
#5674=DIRECTION('',(-3.46944695195361E-16,1.,0.));
#5675=DIRECTION('',(0.,0.,-1.));
#5676=DIRECTION('center_axis',(0.,0.,-1.));
#5677=DIRECTION('ref_axis',(1.,0.,0.));
#5678=DIRECTION('center_axis',(3.46944695195361E-16,-1.,0.));
#5679=DIRECTION('ref_axis',(1.,3.46944695195361E-16,0.));
#5680=DIRECTION('center_axis',(6.088865147686E-17,1.,0.));
#5681=DIRECTION('ref_axis',(-1.,6.088865147686E-17,0.));
#5682=DIRECTION('center_axis',(0.,-1.,0.));
#5683=DIRECTION('ref_axis',(0.,0.,-1.));
#5684=DIRECTION('center_axis',(3.46944695195361E-16,-1.,0.));
#5685=DIRECTION('ref_axis',(1.,3.46944695195361E-16,0.));
#5686=DIRECTION('center_axis',(0.,-1.,0.));
#5687=DIRECTION('ref_axis',(0.,0.,-1.));
#5688=DIRECTION('center_axis',(6.088865147686E-17,1.,0.));
#5689=DIRECTION('ref_axis',(-1.,6.088865147686E-17,0.));
#5690=DIRECTION('center_axis',(1.,0.,0.));
#5691=DIRECTION('ref_axis',(0.,0.,-1.));
#5692=DIRECTION('center_axis',(-1.,0.,0.));
#5693=DIRECTION('ref_axis',(0.,0.,1.));
#5694=DIRECTION('center_axis',(-1.,6.088865147686E-17,0.));
#5695=DIRECTION('ref_axis',(-6.088865147686E-17,-1.,0.));
#5696=DIRECTION('center_axis',(-1.,0.,0.));
#5697=DIRECTION('ref_axis',(0.,0.,1.));
#5698=DIRECTION('center_axis',(0.,-1.,0.));
#5699=DIRECTION('ref_axis',(0.,0.,-1.));
#5700=DIRECTION('center_axis',(0.,0.,-1.));
#5701=DIRECTION('ref_axis',(-1.,0.,0.));
#5702=DIRECTION('center_axis',(6.088865147686E-17,1.,0.));
#5703=DIRECTION('ref_axis',(-1.,0.,0.));
#5704=DIRECTION('center_axis',(0.,0.,-1.));
#5705=DIRECTION('ref_axis',(-1.,0.,0.));
#5706=DIRECTION('center_axis',(0.,0.,1.));
#5707=DIRECTION('ref_axis',(1.,0.,0.));
#5708=DIRECTION('center_axis',(0.,0.,-1.));
#5709=DIRECTION('ref_axis',(-1.,0.,0.));
#5710=DIRECTION('center_axis',(-3.46944695195361E-16,1.,0.));
#5711=DIRECTION('ref_axis',(-1.,-3.46944695195361E-16,0.));
#5712=DIRECTION('center_axis',(6.088865147686E-17,1.,0.));
#5713=DIRECTION('ref_axis',(-1.,6.088865147686E-17,0.));
#5714=DIRECTION('center_axis',(0.,-1.,0.));
#5715=DIRECTION('ref_axis',(0.,0.,-1.));
#5716=DIRECTION('center_axis',(0.,0.,1.));
#5717=DIRECTION('ref_axis',(1.,0.,0.));
#5718=DIRECTION('center_axis',(0.,0.,-1.));
#5719=DIRECTION('ref_axis',(-1.,0.,0.));
#5720=DIRECTION('center_axis',(0.,-1.,0.));
#5721=DIRECTION('ref_axis',(0.,0.,-1.));
#5722=DIRECTION('center_axis',(-1.,0.,0.));
#5723=DIRECTION('ref_axis',(0.,0.,-1.));
#5724=DIRECTION('center_axis',(6.088865147686E-17,1.,0.));
#5725=DIRECTION('ref_axis',(-1.,0.,0.));
#5726=DIRECTION('center_axis',(-1.,0.,0.));
#5727=DIRECTION('ref_axis',(0.,0.,-1.));
#5728=DIRECTION('center_axis',(1.,0.,0.));
#5729=DIRECTION('ref_axis',(0.,0.,-1.));
#5730=DIRECTION('center_axis',(-1.,6.088865147686E-17,0.));
#5731=DIRECTION('ref_axis',(-6.088865147686E-17,-1.,0.));
#5732=DIRECTION('center_axis',(-1.,0.,0.));
#5733=DIRECTION('ref_axis',(0.,0.,1.));
#5734=DIRECTION('center_axis',(0.,0.,1.));
#5735=DIRECTION('ref_axis',(1.,0.,0.));
#5736=DIRECTION('center_axis',(-0.258819045102525,-0.965925826289067,5.8928555905964E-16));
#5737=DIRECTION('ref_axis',(0.965925826289067,-0.258819045102525,-3.84362793942457E-32));
#5738=DIRECTION('center_axis',(-0.258819045102524,-0.965925826289067,0.));
#5739=DIRECTION('ref_axis',(0.965925826289067,-0.258819045102524,0.));
#5740=DIRECTION('center_axis',(-0.258819045102523,-0.965925826289068,-5.61224341961558E-17));
#5741=DIRECTION('ref_axis',(0.965925826289068,-0.258819045102523,-2.72649669415818E-33));
#5742=DIRECTION('center_axis',(0.,0.,1.));
#5743=DIRECTION('ref_axis',(-0.258819045102525,-0.965925826289067,0.));
#5744=DIRECTION('center_axis',(0.258819045102526,0.965925826289067,4.48979473569252E-16));
#5745=DIRECTION('ref_axis',(-0.965925826289067,0.258819045102526,-1.81510300540188E-31));
#5746=DIRECTION('center_axis',(0.258819045102525,0.965925826289067,0.));
#5747=DIRECTION('ref_axis',(-0.965925826289067,0.258819045102525,0.));
#5748=DIRECTION('center_axis',(0.,0.,-1.));
#5749=DIRECTION('ref_axis',(1.,-1.22464679914735E-16,0.));
#5750=DIRECTION('center_axis',(-1.,0.,0.));
#5751=DIRECTION('ref_axis',(0.,0.,1.));
#5752=DIRECTION('center_axis',(-1.,0.,0.));
#5753=DIRECTION('ref_axis',(0.,0.,1.));
#5754=DIRECTION('center_axis',(1.,0.,0.));
#5755=DIRECTION('ref_axis',(0.,0.,-1.));
#5756=DIRECTION('center_axis',(-1.,0.,0.));
#5757=DIRECTION('ref_axis',(0.,0.,1.));
#5758=DIRECTION('center_axis',(-1.,6.088865147686E-17,0.));
#5759=DIRECTION('ref_axis',(-6.088865147686E-17,-1.,0.));
#5760=DIRECTION('center_axis',(-1.,0.,0.));
#5761=DIRECTION('ref_axis',(0.,0.,1.));
#5762=DIRECTION('center_axis',(0.,-1.,0.));
#5763=DIRECTION('ref_axis',(0.,0.,-1.));
#5764=DIRECTION('center_axis',(0.,0.,1.));
#5765=DIRECTION('ref_axis',(1.,0.,0.));
#5766=DIRECTION('center_axis',(6.088865147686E-17,1.,0.));
#5767=DIRECTION('ref_axis',(-1.,0.,0.));
#5768=DIRECTION('center_axis',(0.,0.,1.));
#5769=DIRECTION('ref_axis',(1.,0.,0.));
#5770=DIRECTION('center_axis',(0.,0.,-1.));
#5771=DIRECTION('ref_axis',(-1.,0.,0.));
#5772=DIRECTION('center_axis',(0.,0.,1.));
#5773=DIRECTION('ref_axis',(1.,0.,0.));
#5774=DIRECTION('center_axis',(0.,0.,-1.));
#5775=DIRECTION('ref_axis',(-1.,0.,0.));
#5776=DIRECTION('center_axis',(0.,0.,1.));
#5777=DIRECTION('ref_axis',(1.,0.,0.));
#5778=DIRECTION('center_axis',(-3.46944695195361E-16,1.,0.));
#5779=DIRECTION('ref_axis',(-1.,-3.46944695195361E-16,0.));
#5780=DIRECTION('center_axis',(0.,-1.,0.));
#5781=DIRECTION('ref_axis',(0.,0.,-1.));
#5782=DIRECTION('center_axis',(6.088865147686E-17,1.,0.));
#5783=DIRECTION('ref_axis',(-1.,6.088865147686E-17,0.));
#5784=DIRECTION('center_axis',(0.,-1.,0.));
#5785=DIRECTION('ref_axis',(0.,0.,-1.));
#5786=DIRECTION('center_axis',(-1.,0.,0.));
#5787=DIRECTION('ref_axis',(0.,0.,-1.));
#5788=DIRECTION('center_axis',(6.088865147686E-17,1.,0.));
#5789=DIRECTION('ref_axis',(-1.,0.,0.));
#5790=DIRECTION('center_axis',(-1.,0.,0.));
#5791=DIRECTION('ref_axis',(0.,0.,-1.));
#5792=DIRECTION('center_axis',(1.,0.,0.));
#5793=DIRECTION('ref_axis',(0.,0.,-1.));
#5794=DIRECTION('center_axis',(-1.,6.088865147686E-17,0.));
#5795=DIRECTION('ref_axis',(-6.088865147686E-17,-1.,0.));
#5796=DIRECTION('center_axis',(-1.,0.,0.));
#5797=DIRECTION('ref_axis',(0.,0.,1.));
#5798=DIRECTION('center_axis',(-0.666666666666667,0.74535599249993,5.78241158658935E-16));
#5799=DIRECTION('ref_axis',(-0.74535599249993,-0.666666666666667,6.22764116085459E-33));
#5800=DIRECTION('center_axis',(0.,0.,-1.));
#5801=DIRECTION('ref_axis',(-1.,0.,0.));
#5802=DIRECTION('center_axis',(-0.258819045102525,-0.965925826289067,0.));
#5803=DIRECTION('ref_axis',(0.965925826289067,-0.258819045102525,0.));
#5804=DIRECTION('center_axis',(0.,0.,-1.));
#5805=DIRECTION('ref_axis',(0.608761429008719,-0.793353340291237,0.));
#5806=DIRECTION('center_axis',(0.547412572866653,-0.836862877099655,-4.74804720598323E-16));
#5807=DIRECTION('ref_axis',(0.836862877099655,0.547412572866653,-7.02765767035438E-33));
#5808=DIRECTION('center_axis',(-0.258819045102524,-0.965925826289067,0.));
#5809=DIRECTION('ref_axis',(0.965925826289067,-0.258819045102524,0.));
#5810=DIRECTION('center_axis',(0.258819045102525,0.965925826289067,0.));
#5811=DIRECTION('ref_axis',(-0.965925826289067,0.258819045102525,0.));
#5812=DIRECTION('center_axis',(0.,0.,1.));
#5813=DIRECTION('ref_axis',(1.,0.,0.));
#5814=DIRECTION('center_axis',(0.,0.,1.));
#5815=DIRECTION('ref_axis',(1.,0.,0.));
#5816=DIRECTION('center_axis',(0.,0.,1.));
#5817=DIRECTION('ref_axis',(1.,0.,0.));
#5818=DIRECTION('center_axis',(0.,0.,1.));
#5819=DIRECTION('ref_axis',(1.,0.,0.));
#5820=DIRECTION('axis',(0.,0.,1.));
#5821=DIRECTION('refdir',(1.,0.,0.));
#5822=DIRECTION('center_axis',(0.,0.,-1.));
#5823=DIRECTION('ref_axis',(-1.,0.,0.));
#5824=DIRECTION('center_axis',(0.,0.,1.));
#5825=DIRECTION('ref_axis',(1.,0.,0.));
#5826=DIRECTION('',(0.,0.,-1.));
#5827=DIRECTION('center_axis',(0.,0.,1.));
#5828=DIRECTION('ref_axis',(1.,0.,0.));
#5829=DIRECTION('center_axis',(0.,0.,-1.));
#5830=DIRECTION('ref_axis',(-1.,0.,0.));
#5831=DIRECTION('center_axis',(0.,0.,1.));
#5832=DIRECTION('ref_axis',(1.,0.,0.));
#5833=DIRECTION('',(0.,0.,-1.));
#5834=DIRECTION('center_axis',(0.,0.,1.));
#5835=DIRECTION('ref_axis',(1.,0.,0.));
#5836=DIRECTION('center_axis',(0.,0.,-1.));
#5837=DIRECTION('ref_axis',(-1.,0.,0.));
#5838=DIRECTION('center_axis',(0.,0.,1.));
#5839=DIRECTION('ref_axis',(1.,0.,0.));
#5840=DIRECTION('',(0.,0.,-1.));
#5841=DIRECTION('center_axis',(0.,0.,1.));
#5842=DIRECTION('ref_axis',(1.,0.,0.));
#5843=DIRECTION('',(0.,0.,-1.));
#5844=DIRECTION('center_axis',(0.,0.,1.));
#5845=DIRECTION('ref_axis',(1.,0.,0.));
#5846=DIRECTION('',(1.,1.30104260698261E-16,0.));
#5847=DIRECTION('center_axis',(0.,0.,1.));
#5848=DIRECTION('ref_axis',(-1.,0.,0.));
#5849=DIRECTION('',(-1.,0.,0.));
#5850=DIRECTION('center_axis',(0.,0.,1.));
#5851=DIRECTION('ref_axis',(1.,0.,0.));
#5852=DIRECTION('',(-1.,0.,0.));
#5853=DIRECTION('center_axis',(0.,0.,1.));
#5854=DIRECTION('ref_axis',(-1.,0.,0.));
#5855=DIRECTION('',(1.,1.30104260698261E-16,0.));
#5856=DIRECTION('center_axis',(-1.30104260698261E-16,1.,0.));
#5857=DIRECTION('ref_axis',(-1.,-1.30104260698261E-16,0.));
#5858=DIRECTION('',(0.,0.,-1.));
#5859=DIRECTION('center_axis',(0.,0.,-1.));
#5860=DIRECTION('ref_axis',(1.,1.22464679914735E-16,0.));
#5861=DIRECTION('',(0.,0.,-1.));
#5862=DIRECTION('center_axis',(0.,-1.,0.));
#5863=DIRECTION('ref_axis',(0.,0.,-1.));
#5864=DIRECTION('axis',(0.,0.,1.));
#5865=DIRECTION('refdir',(1.,0.,0.));
#5866=DIRECTION('center_axis',(0.,0.,1.));
#5867=DIRECTION('ref_axis',(1.,0.,0.));
#5868=DIRECTION('center_axis',(0.,0.,1.));
#5869=DIRECTION('ref_axis',(1.,0.,0.));
#5870=DIRECTION('center_axis',(0.,0.,1.));
#5871=DIRECTION('ref_axis',(1.,0.,0.));
#5872=DIRECTION('',(0.707106781186545,8.6595605623549E-17,-0.70710678118655));
#5873=DIRECTION('center_axis',(0.,0.,-1.));
#5874=DIRECTION('ref_axis',(1.,0.,0.));
#5875=DIRECTION('center_axis',(0.,0.,1.));
#5876=DIRECTION('ref_axis',(1.,0.,0.));
#5877=DIRECTION('center_axis',(0.,0.,1.));
#5878=DIRECTION('ref_axis',(1.,0.,0.));
#5879=DIRECTION('center_axis',(0.,0.,1.));
#5880=DIRECTION('ref_axis',(1.,0.,0.));
#5881=DIRECTION('',(0.707106781186545,8.6595605623549E-17,-0.70710678118655));
#5882=DIRECTION('center_axis',(0.,0.,-1.));
#5883=DIRECTION('ref_axis',(1.,0.,0.));
#5884=DIRECTION('center_axis',(0.,0.,-1.));
#5885=DIRECTION('ref_axis',(-1.,0.,0.));
#5886=DIRECTION('center_axis',(0.,0.,-1.));
#5887=DIRECTION('ref_axis',(1.,0.,0.));
#5888=DIRECTION('',(-0.707106781186551,8.65956056235498E-17,0.707106781186544));
#5889=DIRECTION('center_axis',(0.,0.,1.));
#5890=DIRECTION('ref_axis',(1.,0.,0.));
#5891=DIRECTION('center_axis',(0.,0.,-1.));
#5892=DIRECTION('ref_axis',(-1.,0.,0.));
#5893=DIRECTION('center_axis',(0.,0.,-1.));
#5894=DIRECTION('ref_axis',(1.,0.,0.));
#5895=DIRECTION('',(-0.707106781186551,8.65956056235497E-17,0.707106781186544));
#5896=DIRECTION('center_axis',(0.,0.,1.));
#5897=DIRECTION('ref_axis',(1.,0.,0.));
#5898=DIRECTION('center_axis',(0.,0.,-1.));
#5899=DIRECTION('ref_axis',(-1.,0.,0.));
#5900=DIRECTION('center_axis',(0.,0.,1.));
#5901=DIRECTION('ref_axis',(1.,0.,0.));
#5902=DIRECTION('',(0.,0.,1.));
#5903=DIRECTION('center_axis',(0.,0.,-1.));
#5904=DIRECTION('ref_axis',(-1.,0.,0.));
#5905=DIRECTION('',(0.,0.,1.));
#5906=DIRECTION('center_axis',(0.,0.,-1.));
#5907=DIRECTION('ref_axis',(1.,0.,0.));
#5908=DIRECTION('center_axis',(0.,0.,-1.));
#5909=DIRECTION('ref_axis',(-1.,0.,0.));
#5910=DIRECTION('center_axis',(0.,0.,1.));
#5911=DIRECTION('ref_axis',(1.,0.,0.));
#5912=DIRECTION('',(0.,0.,1.));
#5913=DIRECTION('center_axis',(0.,0.,-1.));
#5914=DIRECTION('ref_axis',(-1.,0.,0.));
#5915=DIRECTION('',(0.,0.,1.));
#5916=DIRECTION('center_axis',(0.,0.,-1.));
#5917=DIRECTION('ref_axis',(1.,0.,0.));
#5918=DIRECTION('center_axis',(0.,0.,1.));
#5919=DIRECTION('ref_axis',(1.,0.,0.));
#5920=DIRECTION('',(-0.613967345345676,-0.789331425225921,0.));
#5921=DIRECTION('',(0.613967345345676,-0.78933142522592,0.));
#5922=DIRECTION('',(1.,1.98254111540207E-16,0.));
#5923=DIRECTION('',(0.984807753012208,0.173648177666931,0.));
#5924=DIRECTION('',(0.984807753012208,-0.173648177666931,0.));
#5925=DIRECTION('',(1.,0.,0.));
#5926=DIRECTION('',(0.,1.,0.));
#5927=DIRECTION('',(-0.944943348295466,0.327233966012321,0.));
#5928=DIRECTION('',(-1.,1.98254111540207E-16,0.));
#5929=DIRECTION('center_axis',(0.,0.,1.));
#5930=DIRECTION('ref_axis',(1.,0.,0.));
#5931=DIRECTION('',(-0.613967345345676,-0.789331425225921,0.));
#5932=DIRECTION('',(-1.,1.98254111540207E-16,0.));
#5933=DIRECTION('',(-0.944943348295466,0.327233966012321,0.));
#5934=DIRECTION('',(0.,1.,0.));
#5935=DIRECTION('',(1.,0.,0.));
#5936=DIRECTION('',(0.984807753012208,-0.173648177666931,0.));
#5937=DIRECTION('',(0.984807753012208,0.173648177666931,0.));
#5938=DIRECTION('',(1.,1.98254111540207E-16,0.));
#5939=DIRECTION('',(0.613967345345676,-0.78933142522592,0.));
#5940=DIRECTION('center_axis',(0.789331425225921,-0.613967345345676,0.));
#5941=DIRECTION('ref_axis',(0.613967345345676,0.789331425225921,0.));
#5942=DIRECTION('',(0.,0.,-1.));
#5943=DIRECTION('',(0.,0.,-1.));
#5944=DIRECTION('center_axis',(0.78933142522592,0.613967345345677,0.));
#5945=DIRECTION('ref_axis',(-0.613967345345677,0.78933142522592,0.));
#5946=DIRECTION('',(0.,0.,-1.));
#5947=DIRECTION('center_axis',(-1.98254111540206E-16,1.,0.));
#5948=DIRECTION('ref_axis',(-1.,-1.98254111540207E-16,0.));
#5949=DIRECTION('',(0.,0.,-1.));
#5950=DIRECTION('center_axis',(-0.173648177666931,0.984807753012208,0.));
#5951=DIRECTION('ref_axis',(-0.984807753012208,-0.173648177666931,0.));
#5952=DIRECTION('',(0.,0.,-1.));
#5953=DIRECTION('center_axis',(0.173648177666931,0.984807753012208,0.));
#5954=DIRECTION('ref_axis',(-0.984807753012208,0.173648177666931,0.));
#5955=DIRECTION('',(0.,0.,-1.));
#5956=DIRECTION('center_axis',(0.,1.,0.));
#5957=DIRECTION('ref_axis',(0.,0.,1.));
#5958=DIRECTION('',(0.,0.,-1.));
#5959=DIRECTION('center_axis',(-1.,0.,0.));
#5960=DIRECTION('ref_axis',(0.,0.,1.));
#5961=DIRECTION('',(0.,0.,-1.));
#5962=DIRECTION('center_axis',(-0.327233966012321,-0.944943348295466,0.));
#5963=DIRECTION('ref_axis',(0.944943348295467,-0.327233966012321,0.));
#5964=DIRECTION('',(0.,0.,-1.));
#5965=DIRECTION('center_axis',(-1.98254111540206E-16,-1.,0.));
#5966=DIRECTION('ref_axis',(1.,-1.98254111540207E-16,0.));
#5967=DIRECTION('center_axis',(0.,0.,1.));
#5968=DIRECTION('ref_axis',(1.,0.,0.));
#5969=DIRECTION('center_axis',(0.,0.,1.));
#5970=DIRECTION('ref_axis',(1.,0.,0.));
#5971=DIRECTION('center_axis',(0.,0.,1.));
#5972=DIRECTION('ref_axis',(1.,0.,0.));
#5973=DIRECTION('center_axis',(0.,0.,1.));
#5974=DIRECTION('ref_axis',(1.,0.,0.));
#5975=DIRECTION('',(0.,0.,1.));
#5976=DIRECTION('',(1.,0.,0.));
#5977=DIRECTION('',(0.,0.,1.));
#5978=DIRECTION('',(0.6091566575904,0.793049914263467,0.));
#5979=DIRECTION('',(0.,0.,1.));
#5980=DIRECTION('',(-1.,0.,0.));
#5981=DIRECTION('',(-1.,0.,0.));
#5982=DIRECTION('',(0.,-0.0293538850747906,-0.999569081870291));
#5983=DIRECTION('',(-1.,0.,0.));
#5984=DIRECTION('',(0.,0.00315510692716888,0.999995022637752));
#5985=DIRECTION('',(-1.,0.,0.));
#5986=DIRECTION('',(0.,9.99200722162641E-16,-1.));
#5987=DIRECTION('',(1.,0.,0.));
#5988=DIRECTION('',(0.,-0.0293538850747948,-0.999569081870291));
#5989=DIRECTION('',(-1.,0.,0.));
#5990=DIRECTION('',(0.,-0.00315510692717049,0.999995022637752));
#5991=DIRECTION('',(1.,0.,0.));
#5992=DIRECTION('',(0.,0.0293538850747874,-0.999569081870291));
#5993=DIRECTION('',(1.,0.,0.));
#5994=DIRECTION('',(0.,0.0293538850747952,-0.999569081870291));
#5995=DIRECTION('',(1.,0.,0.));
#5996=DIRECTION('',(0.,6.66133814775094E-16,-1.));
#5997=CARTESIAN_POINT('',(0.,0.,0.));
#5998=CARTESIAN_POINT('',(0.,0.,0.));
#5999=CARTESIAN_POINT('',(0.,0.,0.));
#6000=CARTESIAN_POINT('Origin',(0.,0.,-50.));
#6001=CARTESIAN_POINT('',(0.,-34.,-44.));
#6002=CARTESIAN_POINT('',(0.,-34.,-56.));
#6003=CARTESIAN_POINT('Origin',(0.,-39.2915026221292,-50.));
#6004=CARTESIAN_POINT('',(0.,34.,-56.));
#6005=CARTESIAN_POINT('Origin',(0.,0.,-56.));
#6006=CARTESIAN_POINT('',(0.,34.,-44.));
#6007=CARTESIAN_POINT('Origin',(0.,39.2915026221292,-50.));
#6008=CARTESIAN_POINT('Origin',(0.,0.,-44.));
#6009=CARTESIAN_POINT('Origin',(33.,41.,-147.));
#6010=CARTESIAN_POINT('',(33.,41.,-152.));
#6011=CARTESIAN_POINT('Origin',(33.,41.,-147.));
#6012=CARTESIAN_POINT('',(34.,41.,-151.));
#6013=CARTESIAN_POINT('Origin',(33.,41.,-151.));
#6014=CARTESIAN_POINT('Origin',(34.,41.,-147.));
#6015=CARTESIAN_POINT('Origin',(34.,41.,-147.));
#6016=CARTESIAN_POINT('',(24.,41.,-152.));
#6017=CARTESIAN_POINT('Origin',(24.,41.,-147.));
#6018=CARTESIAN_POINT('',(34.,41.,-152.));
#6019=CARTESIAN_POINT('Origin',(33.,-41.,-147.));
#6020=CARTESIAN_POINT('',(33.,-41.,-152.));
#6021=CARTESIAN_POINT('Origin',(33.,-41.,-147.));
#6022=CARTESIAN_POINT('',(34.,-41.,-151.));
#6023=CARTESIAN_POINT('Origin',(33.,-41.,-151.));
#6024=CARTESIAN_POINT('Origin',(34.,-41.,-147.));
#6025=CARTESIAN_POINT('Origin',(34.,-41.,-147.));
#6026=CARTESIAN_POINT('',(24.,-41.,-152.));
#6027=CARTESIAN_POINT('Origin',(24.,-41.,-147.));
#6028=CARTESIAN_POINT('',(34.,-41.,-152.));
#6029=CARTESIAN_POINT('Origin',(0.,0.,-165.));
#6030=CARTESIAN_POINT('',(0.,5.,-165.));
#6031=CARTESIAN_POINT('',(0.,-5.,-165.));
#6032=CARTESIAN_POINT('Origin',(0.,0.,-165.));
#6033=CARTESIAN_POINT('',(0.,-5.,-153.));
#6034=CARTESIAN_POINT('',(0.,-5.,-165.));
#6035=CARTESIAN_POINT('',(0.,5.,-153.));
#6036=CARTESIAN_POINT('Origin',(0.,0.,-153.));
#6037=CARTESIAN_POINT('',(0.,5.,-165.));
#6038=CARTESIAN_POINT('Origin',(24.,-67.,-127.));
#6039=CARTESIAN_POINT('',(24.,-67.,-132.));
#6040=CARTESIAN_POINT('Origin',(24.,-67.,-127.));
#6041=CARTESIAN_POINT('',(16.,-67.,-132.));
#6042=CARTESIAN_POINT('',(24.,-67.,-132.));
#6043=CARTESIAN_POINT('Origin',(16.,-67.,-127.));
#6044=CARTESIAN_POINT('Origin',(24.,67.,-127.));
#6045=CARTESIAN_POINT('',(24.,67.,-132.));
#6046=CARTESIAN_POINT('Origin',(24.,67.,-127.));
#6047=CARTESIAN_POINT('',(16.,67.,-132.));
#6048=CARTESIAN_POINT('',(24.,67.,-132.));
#6049=CARTESIAN_POINT('Origin',(16.,67.,-127.));
#6050=CARTESIAN_POINT('Origin',(0.,0.,54.));
#6051=CARTESIAN_POINT('',(0.,-23.5,-46.));
#6052=CARTESIAN_POINT('',(0.,23.5,-46.));
#6053=CARTESIAN_POINT('Origin',(0.,0.,-46.));
#6054=CARTESIAN_POINT('',(0.,-23.5,-9.18183714823662E-16));
#6055=CARTESIAN_POINT('',(0.,-23.5,54.));
#6056=CARTESIAN_POINT('',(0.,23.5,0.));
#6057=CARTESIAN_POINT('Origin',(0.,0.,-9.18183714823662E-16));
#6058=CARTESIAN_POINT('',(0.,23.5,54.));
#6059=CARTESIAN_POINT('Origin',(0.,0.,54.));
#6060=CARTESIAN_POINT('',(0.,-22.,-63.));
#6061=CARTESIAN_POINT('',(0.,22.,-63.));
#6062=CARTESIAN_POINT('Origin',(0.,0.,-63.));
#6063=CARTESIAN_POINT('',(0.,-22.,-46.));
#6064=CARTESIAN_POINT('',(0.,-22.,54.));
#6065=CARTESIAN_POINT('',(0.,22.,-46.));
#6066=CARTESIAN_POINT('Origin',(0.,0.,-46.));
#6067=CARTESIAN_POINT('',(0.,22.,54.));
#6068=CARTESIAN_POINT('Origin',(0.,0.,54.));
#6069=CARTESIAN_POINT('',(0.,-15.,-71.));
#6070=CARTESIAN_POINT('',(0.,15.,-71.));
#6071=CARTESIAN_POINT('Origin',(0.,0.,-71.));
#6072=CARTESIAN_POINT('',(0.,-15.,-63.));
#6073=CARTESIAN_POINT('',(0.,-15.,54.));
#6074=CARTESIAN_POINT('',(0.,15.,-63.));
#6075=CARTESIAN_POINT('Origin',(0.,0.,-63.));
#6076=CARTESIAN_POINT('',(0.,15.,54.));
#6077=CARTESIAN_POINT('Origin',(0.,0.,54.));
#6078=CARTESIAN_POINT('',(0.,-55.,-71.));
#6079=CARTESIAN_POINT('',(0.,55.,-71.));
#6080=CARTESIAN_POINT('Origin',(0.,0.,-71.));
#6081=CARTESIAN_POINT('',(0.,55.,-63.));
#6082=CARTESIAN_POINT('',(0.,55.,54.));
#6083=CARTESIAN_POINT('',(0.,-55.,-63.));
#6084=CARTESIAN_POINT('Origin',(0.,0.,-63.));
#6085=CARTESIAN_POINT('',(0.,-55.,54.));
#6086=CARTESIAN_POINT('Origin',(0.,0.,54.));
#6087=CARTESIAN_POINT('',(0.,-34.,-63.));
#6088=CARTESIAN_POINT('',(0.,34.,-63.));
#6089=CARTESIAN_POINT('Origin',(0.,0.,-63.));
#6090=CARTESIAN_POINT('',(0.,34.,54.));
#6091=CARTESIAN_POINT('',(0.,-34.,54.));
#6092=CARTESIAN_POINT('Origin',(0.,0.,54.));
#6093=CARTESIAN_POINT('',(0.,34.,-14.));
#6094=CARTESIAN_POINT('',(0.,34.,54.));
#6095=CARTESIAN_POINT('',(0.,-34.,-14.));
#6096=CARTESIAN_POINT('Origin',(0.,0.,-14.));
#6097=CARTESIAN_POINT('',(0.,-34.,54.));
#6098=CARTESIAN_POINT('Origin',(24.,-67.,-127.));
#6099=CARTESIAN_POINT('',(24.,-20.,-153.));
#6100=CARTESIAN_POINT('',(24.,-20.,-165.));
#6101=CARTESIAN_POINT('',(24.,-20.,-153.));
#6102=CARTESIAN_POINT('',(24.,20.,-153.));
#6103=CARTESIAN_POINT('',(24.,-20.,-153.));
#6104=CARTESIAN_POINT('',(24.,20.,-165.));
#6105=CARTESIAN_POINT('',(24.,20.,-153.));
#6106=CARTESIAN_POINT('',(24.,46.,-165.));
#6107=CARTESIAN_POINT('',(24.,-46.,-165.));
#6108=CARTESIAN_POINT('',(24.,74.4030339164196,-133.7227292696));
#6109=CARTESIAN_POINT('',(24.,74.4030339164196,-133.7227292696));
#6110=CARTESIAN_POINT('',(24.,74.426181142428,-120.302848841496));
#6111=CARTESIAN_POINT('Origin',(24.,67.,-127.));
#6112=CARTESIAN_POINT('',(24.,48.,-91.));
#6113=CARTESIAN_POINT('',(24.,48.,-91.));
#6114=CARTESIAN_POINT('',(24.,48.,-71.));
#6115=CARTESIAN_POINT('',(24.,48.,-71.));
#6116=CARTESIAN_POINT('',(24.,29.,-71.));
#6117=CARTESIAN_POINT('',(24.,48.,-71.));
#6118=CARTESIAN_POINT('',(24.,29.,-149.3613646348));
#6119=CARTESIAN_POINT('',(24.,29.,-71.));
#6120=CARTESIAN_POINT('',(24.,21.,-149.3613646348));
#6121=CARTESIAN_POINT('',(24.,29.,-149.3613646348));
#6122=CARTESIAN_POINT('',(24.,21.,-71.));
#6123=CARTESIAN_POINT('',(24.,21.,-71.));
#6124=CARTESIAN_POINT('',(24.,-21.,-71.));
#6125=CARTESIAN_POINT('',(24.,48.,-71.));
#6126=CARTESIAN_POINT('',(24.,-21.,-149.3613646348));
#6127=CARTESIAN_POINT('',(24.,-21.,-71.));
#6128=CARTESIAN_POINT('',(24.,-29.,-149.3613646348));
#6129=CARTESIAN_POINT('',(24.,-29.,-149.3613646348));
#6130=CARTESIAN_POINT('',(24.,-29.,-71.));
#6131=CARTESIAN_POINT('',(24.,-29.,-71.));
#6132=CARTESIAN_POINT('',(24.,-48.,-71.));
#6133=CARTESIAN_POINT('',(24.,48.,-71.));
#6134=CARTESIAN_POINT('',(24.,-48.,-91.));
#6135=CARTESIAN_POINT('',(24.,-48.,-71.));
#6136=CARTESIAN_POINT('',(24.,-74.426181142428,-120.302848841496));
#6137=CARTESIAN_POINT('',(24.,-48.,-91.));
#6138=CARTESIAN_POINT('',(24.,-74.4030339164196,-133.7227292696));
#6139=CARTESIAN_POINT('Origin',(24.,-67.,-127.));
#6140=CARTESIAN_POINT('',(24.,-46.,-165.));
#6141=CARTESIAN_POINT('',(24.,-74.4030339164196,-133.7227292696));
#6142=CARTESIAN_POINT('',(24.,-46.,-165.));
#6143=CARTESIAN_POINT('Origin',(0.,93.,313.849585789117));
#6144=CARTESIAN_POINT('',(0.,31.5,6.12303176911193E-17));
#6145=CARTESIAN_POINT('',(0.,0.,176.4));
#6146=CARTESIAN_POINT('',(0.,55.,-63.));
#6147=CARTESIAN_POINT('',(0.,15.,-71.));
#6148=CARTESIAN_POINT('',(0.,22.,-63.));
#6149=CARTESIAN_POINT('',(0.,23.5,-46.));
#6150=CARTESIAN_POINT('',(0.,31.5,6.12303176911193E-17));
#6151=CARTESIAN_POINT('Origin',(-24.,20.,-153.));
#6152=CARTESIAN_POINT('',(16.,-20.,-153.));
#6153=CARTESIAN_POINT('',(16.,-19.,-153.));
#6154=CARTESIAN_POINT('',(16.,-67.,-153.));
#6155=CARTESIAN_POINT('',(23.,-19.,-153.));
#6156=CARTESIAN_POINT('',(23.,-19.,-153.));
#6157=CARTESIAN_POINT('',(23.,19.,-153.));
#6158=CARTESIAN_POINT('',(23.,19.,-153.));
#6159=CARTESIAN_POINT('',(16.,19.,-153.));
#6160=CARTESIAN_POINT('',(-24.,19.,-153.));
#6161=CARTESIAN_POINT('',(16.,20.,-153.));
#6162=CARTESIAN_POINT('',(16.,-67.,-153.));
#6163=CARTESIAN_POINT('',(-24.,20.,-153.));
#6164=CARTESIAN_POINT('',(-24.,-20.,-153.));
#6165=CARTESIAN_POINT('Origin',(24.,46.,-165.));
#6166=CARTESIAN_POINT('',(16.,-46.,-165.));
#6167=CARTESIAN_POINT('',(16.,-20.,-165.));
#6168=CARTESIAN_POINT('',(16.,46.,-165.));
#6169=CARTESIAN_POINT('',(-24.,-20.,-165.));
#6170=CARTESIAN_POINT('',(24.,-46.,-165.));
#6171=CARTESIAN_POINT('Origin',(0.,15.,-71.));
#6172=CARTESIAN_POINT('',(0.,15.,-71.));
#6173=CARTESIAN_POINT('',(44.,-29.,-71.));
#6174=CARTESIAN_POINT('',(44.,-29.,-71.));
#6175=CARTESIAN_POINT('',(44.,-21.,-71.));
#6176=CARTESIAN_POINT('',(44.,-29.,-71.));
#6177=CARTESIAN_POINT('',(44.,-21.,-71.));
#6178=CARTESIAN_POINT('',(44.,21.,-71.));
#6179=CARTESIAN_POINT('',(44.,21.,-71.));
#6180=CARTESIAN_POINT('',(44.,29.,-71.));
#6181=CARTESIAN_POINT('',(44.,29.,-71.));
#6182=CARTESIAN_POINT('',(44.,29.,-71.));
#6183=CARTESIAN_POINT('',(16.,48.,-71.));
#6184=CARTESIAN_POINT('',(24.,48.,-71.));
#6185=CARTESIAN_POINT('',(16.,-48.,-71.));
#6186=CARTESIAN_POINT('',(16.,48.,-71.));
#6187=CARTESIAN_POINT('',(24.,-48.,-71.));
#6188=CARTESIAN_POINT('Origin',(0.,31.5,6.12303176911193E-17));
#6189=CARTESIAN_POINT('',(0.,-31.5,6.12303176911193E-17));
#6190=CARTESIAN_POINT('Origin',(0.,0.,6.09863722023096E-17));
#6191=CARTESIAN_POINT('',(0.,31.5,6.12303176911193E-17));
#6192=CARTESIAN_POINT('Origin',(0.,0.,-14.));
#6193=CARTESIAN_POINT('',(0.,0.,176.4));
#6194=CARTESIAN_POINT('Origin',(0.,55.,-63.));
#6195=CARTESIAN_POINT('',(0.,55.,-63.));
#6196=CARTESIAN_POINT('Origin',(0.,22.,-63.));
#6197=CARTESIAN_POINT('',(0.,22.,-63.));
#6198=CARTESIAN_POINT('Origin',(0.,23.5,-46.));
#6199=CARTESIAN_POINT('',(0.,23.5,-46.));
#6200=CARTESIAN_POINT('Origin',(16.,-67.,-127.));
#6201=CARTESIAN_POINT('',(16.,-20.,-127.));
#6202=CARTESIAN_POINT('',(16.,-74.4030339164196,-133.7227292696));
#6203=CARTESIAN_POINT('',(16.,-74.4030339164196,-133.7227292696));
#6204=CARTESIAN_POINT('',(16.,-74.426181142428,-120.302848841496));
#6205=CARTESIAN_POINT('Origin',(16.,-67.,-127.));
#6206=CARTESIAN_POINT('',(16.,-48.,-91.));
#6207=CARTESIAN_POINT('',(16.,-48.,-91.));
#6208=CARTESIAN_POINT('',(16.,-48.,-71.));
#6209=CARTESIAN_POINT('',(16.,48.,-91.));
#6210=CARTESIAN_POINT('',(16.,48.,-71.));
#6211=CARTESIAN_POINT('',(16.,74.426181142428,-120.302848841496));
#6212=CARTESIAN_POINT('',(16.,48.,-91.));
#6213=CARTESIAN_POINT('',(16.,74.4030339164196,-133.7227292696));
#6214=CARTESIAN_POINT('Origin',(16.,67.,-127.));
#6215=CARTESIAN_POINT('',(16.,46.,-165.));
#6216=CARTESIAN_POINT('',(16.,74.4030339164196,-133.7227292696));
#6217=CARTESIAN_POINT('',(16.,20.,-165.));
#6218=CARTESIAN_POINT('',(16.,46.,-165.));
#6219=CARTESIAN_POINT('',(16.,20.,-127.));
#6220=CARTESIAN_POINT('',(16.,-67.,-153.));
#6221=CARTESIAN_POINT('Origin',(24.,-48.,-71.));
#6222=CARTESIAN_POINT('',(24.,-48.,-91.));
#6223=CARTESIAN_POINT('Origin',(24.,-48.,-91.));
#6224=CARTESIAN_POINT('',(24.,-74.426181142428,-120.302848841496));
#6225=CARTESIAN_POINT('Origin',(24.,-67.,-127.));
#6226=CARTESIAN_POINT('',(24.,-74.4030339164196,-133.7227292696));
#6227=CARTESIAN_POINT('Origin',(24.,-74.4030339164196,-133.7227292696));
#6228=CARTESIAN_POINT('Origin',(24.,46.,-165.));
#6229=CARTESIAN_POINT('',(-24.,20.,-165.));
#6230=CARTESIAN_POINT('',(24.,46.,-165.));
#6231=CARTESIAN_POINT('Origin',(24.,74.4030339164196,-133.7227292696));
#6232=CARTESIAN_POINT('',(24.,74.4030339164196,-133.7227292696));
#6233=CARTESIAN_POINT('Origin',(24.,67.,-127.));
#6234=CARTESIAN_POINT('',(24.,74.426181142428,-120.302848841496));
#6235=CARTESIAN_POINT('Origin',(24.,48.,-91.));
#6236=CARTESIAN_POINT('',(24.,48.,-91.));
#6237=CARTESIAN_POINT('Origin',(24.,48.,-71.));
#6238=CARTESIAN_POINT('Origin',(44.,29.,-71.));
#6239=CARTESIAN_POINT('',(44.,21.,-71.));
#6240=CARTESIAN_POINT('',(44.,29.,-71.));
#6241=CARTESIAN_POINT('Origin',(24.,29.,-71.));
#6242=CARTESIAN_POINT('Origin',(24.,21.,-71.));
#6243=CARTESIAN_POINT('Origin',(44.,-29.,-71.));
#6244=CARTESIAN_POINT('',(44.,-21.,-71.));
#6245=CARTESIAN_POINT('',(44.,-29.,-71.));
#6246=CARTESIAN_POINT('Origin',(24.,-29.,-71.));
#6247=CARTESIAN_POINT('Origin',(24.,-21.,-71.));
#6248=CARTESIAN_POINT('Origin',(-24.,-20.,-153.));
#6249=CARTESIAN_POINT('Origin',(-24.,20.,-153.));
#6250=CARTESIAN_POINT('Origin',(23.,-19.,-153.));
#6251=CARTESIAN_POINT('',(0.,19.,-153.));
#6252=CARTESIAN_POINT('',(23.,19.,-153.));
#6253=CARTESIAN_POINT('',(0.,-19.,-153.));
#6254=CARTESIAN_POINT('',(0.,-19.,-153.));
#6255=CARTESIAN_POINT('',(0.,-19.,-153.));
#6256=CARTESIAN_POINT('',(23.,-19.,-153.));
#6257=CARTESIAN_POINT('Origin',(23.,-19.,-165.));
#6258=CARTESIAN_POINT('',(0.,19.,-165.));
#6259=CARTESIAN_POINT('',(0.,-19.,-165.));
#6260=CARTESIAN_POINT('',(23.,19.,-165.));
#6261=CARTESIAN_POINT('',(23.,19.,-165.));
#6262=CARTESIAN_POINT('',(23.,-19.,-165.));
#6263=CARTESIAN_POINT('',(23.,19.,-165.));
#6264=CARTESIAN_POINT('',(0.,-19.,-165.));
#6265=CARTESIAN_POINT('',(23.,-19.,-165.));
#6266=CARTESIAN_POINT('',(0.,-19.,-165.));
#6267=CARTESIAN_POINT('Origin',(23.,19.,-165.));
#6268=CARTESIAN_POINT('',(23.,-19.,-165.));
#6269=CARTESIAN_POINT('',(23.,19.,-165.));
#6270=CARTESIAN_POINT('Origin',(23.,-19.,-165.));
#6271=CARTESIAN_POINT('',(0.,-19.,-165.));
#6272=CARTESIAN_POINT('Origin',(23.,19.,-165.));
#6273=CARTESIAN_POINT('',(0.,19.,-165.));
#6274=CARTESIAN_POINT('Origin',(0.,93.,313.849585789117));
#6275=CARTESIAN_POINT('Origin',(0.,93.,313.849585789117));
#6276=CARTESIAN_POINT('Origin',(0.,93.,313.849585789117));
#6277=CARTESIAN_POINT('Origin',(34.,-41.,-147.));
#6278=CARTESIAN_POINT('Origin',(34.,41.,-147.));
#6279=CARTESIAN_POINT('',(0.,0.,0.));
#6280=CARTESIAN_POINT('',(0.,0.,0.));
#6281=CARTESIAN_POINT('Origin',(0.,0.,67.));
#6282=CARTESIAN_POINT('',(-6.,-7.34788079488412E-16,-68.));
#6283=CARTESIAN_POINT('Origin',(0.,0.,-68.));
#6284=CARTESIAN_POINT('',(-6.,-7.34788079488412E-16,-148.));
#6285=CARTESIAN_POINT('',(-6.,-7.34788079488412E-16,67.));
#6286=CARTESIAN_POINT('Origin',(0.,0.,-148.));
#6287=CARTESIAN_POINT('Origin',(0.,0.,67.));
#6288=CARTESIAN_POINT('',(-5.,-6.12323399573677E-16,-148.));
#6289=CARTESIAN_POINT('Origin',(0.,0.,-148.));
#6290=CARTESIAN_POINT('',(-5.,-6.12323399573677E-16,-170.));
#6291=CARTESIAN_POINT('',(-5.,-6.12323399573677E-16,67.));
#6292=CARTESIAN_POINT('Origin',(0.,0.,-170.));
#6293=CARTESIAN_POINT('Origin',(0.,0.,67.));
#6294=CARTESIAN_POINT('',(-10.,-1.22464679914735E-15,-14.));
#6295=CARTESIAN_POINT('Origin',(0.,0.,-14.));
#6296=CARTESIAN_POINT('',(-10.,-1.22464679914735E-15,-60.));
#6297=CARTESIAN_POINT('',(-10.,-1.22464679914735E-15,67.));
#6298=CARTESIAN_POINT('',(-8.1689471959571,-5.76786803850996,-60.));
#6299=CARTESIAN_POINT('Origin',(0.,0.,-60.));
#6300=CARTESIAN_POINT('',(0.910646649047397,-9.95844981312749,-60.));
#6301=CARTESIAN_POINT('Origin',(0.,0.,-60.));
#6302=CARTESIAN_POINT('',(9.07959384500449,-4.19058177461752,-60.));
#6303=CARTESIAN_POINT('Origin',(0.,0.,-60.));
#6304=CARTESIAN_POINT('',(8.1689471959571,5.76786803850996,-60.));
#6305=CARTESIAN_POINT('Origin',(0.,0.,-60.));
#6306=CARTESIAN_POINT('',(-0.910646649047399,9.95844981312748,-60.));
#6307=CARTESIAN_POINT('Origin',(0.,0.,-60.));
#6308=CARTESIAN_POINT('',(-9.0795938450045,4.19058177461752,-60.));
#6309=CARTESIAN_POINT('Origin',(0.,0.,-60.));
#6310=CARTESIAN_POINT('Origin',(0.,0.,-60.));
#6311=CARTESIAN_POINT('Origin',(0.,0.,67.));
#6312=CARTESIAN_POINT('',(-14.,-1.71450551880629E-15,0.));
#6313=CARTESIAN_POINT('Origin',(0.,0.,0.));
#6314=CARTESIAN_POINT('',(-14.,-1.71450551880629E-15,-14.));
#6315=CARTESIAN_POINT('',(-14.,-1.71450551880629E-15,67.));
#6316=CARTESIAN_POINT('Origin',(0.,0.,-14.));
#6317=CARTESIAN_POINT('Origin',(0.,0.,0.));
#6318=CARTESIAN_POINT('',(6.92820323027551,1.73472347597681E-15,0.));
#6319=CARTESIAN_POINT('',(3.46410161513776,6.,0.));
#6320=CARTESIAN_POINT('',(6.92820323027551,1.73472347597681E-15,0.));
#6321=CARTESIAN_POINT('',(3.46410161513776,-6.,0.));
#6322=CARTESIAN_POINT('',(3.46410161513776,-6.,0.));
#6323=CARTESIAN_POINT('',(-3.46410161513776,-6.,0.));
#6324=CARTESIAN_POINT('',(-3.46410161513776,-6.,0.));
#6325=CARTESIAN_POINT('',(-6.92820323027551,6.71609035746146E-16,0.));
#6326=CARTESIAN_POINT('',(-6.92820323027551,6.71609035746146E-16,0.));
#6327=CARTESIAN_POINT('',(-3.46410161513776,6.,0.));
#6328=CARTESIAN_POINT('',(-3.46410161513776,6.,0.));
#6329=CARTESIAN_POINT('',(3.46410161513776,6.,0.));
#6330=CARTESIAN_POINT('Origin',(0.,14.,-14.));
#6331=CARTESIAN_POINT('Origin',(3.46410161513776,-6.,-10.));
#6332=CARTESIAN_POINT('',(6.92820323027551,1.73472347597681E-15,-10.));
#6333=CARTESIAN_POINT('',(6.92820323027551,1.73472347597681E-15,-10.));
#6334=CARTESIAN_POINT('',(3.46410161513776,-6.,-10.));
#6335=CARTESIAN_POINT('',(3.46410161513776,-6.,-10.));
#6336=CARTESIAN_POINT('',(3.46410161513776,-6.,-10.));
#6337=CARTESIAN_POINT('Origin',(-3.46410161513776,-6.,-10.));
#6338=CARTESIAN_POINT('',(-3.46410161513776,-6.,-10.));
#6339=CARTESIAN_POINT('',(-3.46410161513776,-6.,-10.));
#6340=CARTESIAN_POINT('',(-3.46410161513776,-6.,-10.));
#6341=CARTESIAN_POINT('Origin',(-6.92820323027551,6.71609035746146E-16,
-10.));
#6342=CARTESIAN_POINT('',(-6.92820323027551,6.71609035746146E-16,-10.));
#6343=CARTESIAN_POINT('',(-6.92820323027551,6.71609035746146E-16,-10.));
#6344=CARTESIAN_POINT('',(-6.92820323027551,6.71609035746146E-16,-10.));
#6345=CARTESIAN_POINT('Origin',(-3.46410161513776,6.,-10.));
#6346=CARTESIAN_POINT('',(-3.46410161513776,6.,-10.));
#6347=CARTESIAN_POINT('',(-3.46410161513776,6.,-10.));
#6348=CARTESIAN_POINT('',(-3.46410161513776,6.,-10.));
#6349=CARTESIAN_POINT('Origin',(3.46410161513776,6.,-10.));
#6350=CARTESIAN_POINT('',(3.46410161513776,6.,-10.));
#6351=CARTESIAN_POINT('',(3.46410161513776,6.,-10.));
#6352=CARTESIAN_POINT('',(3.46410161513776,6.,-10.));
#6353=CARTESIAN_POINT('Origin',(6.92820323027551,1.73472347597681E-15,-10.));
#6354=CARTESIAN_POINT('',(6.92820323027551,1.73472347597681E-15,-10.));
#6355=CARTESIAN_POINT('Origin',(3.46410161513776,-6.,-10.));
#6356=CARTESIAN_POINT('Origin',(-16.3378943919142,-11.5357360770199,-68.));
#6357=CARTESIAN_POINT('',(6.66016032936793,-9.43268772516334,-68.));
#6358=CARTESIAN_POINT('',(-4.83886703127313,-10.4842119010916,-68.));
#6359=CARTESIAN_POINT('',(6.66016032936793,-9.43268772516334,-68.));
#6360=CARTESIAN_POINT('',(-11.4990273606411,-1.0515241759283,-68.));
#6361=CARTESIAN_POINT('',(-4.83886703127313,-10.4842119010916,-68.));
#6362=CARTESIAN_POINT('',(-6.66016032936793,9.43268772516333,-68.));
#6363=CARTESIAN_POINT('',(-11.4990273606411,-1.0515241759283,-68.));
#6364=CARTESIAN_POINT('',(4.83886703127313,10.4842119010916,-68.));
#6365=CARTESIAN_POINT('',(-6.66016032936793,9.43268772516333,-68.));
#6366=CARTESIAN_POINT('',(11.4990273606411,1.05152417592829,-68.));
#6367=CARTESIAN_POINT('',(4.83886703127313,10.4842119010916,-68.));
#6368=CARTESIAN_POINT('',(11.4990273606411,1.05152417592829,-68.));
#6369=CARTESIAN_POINT('Origin',(-16.3378943919142,-11.5357360770199,-60.));
#6370=CARTESIAN_POINT('',(-6.66016032936793,9.43268772516333,-60.));
#6371=CARTESIAN_POINT('',(-11.4990273606411,-1.0515241759283,-60.));
#6372=CARTESIAN_POINT('',(-6.66016032936793,9.43268772516333,-60.));
#6373=CARTESIAN_POINT('Origin',(-16.3378943919142,-11.5357360770199,-60.));
#6374=CARTESIAN_POINT('',(4.83886703127313,10.4842119010916,-60.));
#6375=CARTESIAN_POINT('',(-6.66016032936793,9.43268772516333,-60.));
#6376=CARTESIAN_POINT('',(4.83886703127313,10.4842119010916,-60.));
#6377=CARTESIAN_POINT('Origin',(-16.3378943919142,-11.5357360770199,-60.));
#6378=CARTESIAN_POINT('',(11.4990273606411,1.05152417592829,-60.));
#6379=CARTESIAN_POINT('',(4.83886703127313,10.4842119010916,-60.));
#6380=CARTESIAN_POINT('',(11.4990273606411,1.05152417592829,-60.));
#6381=CARTESIAN_POINT('Origin',(-16.3378943919142,-11.5357360770199,-60.));
#6382=CARTESIAN_POINT('',(6.66016032936793,-9.43268772516334,-60.));
#6383=CARTESIAN_POINT('',(11.4990273606411,1.05152417592829,-60.));
#6384=CARTESIAN_POINT('',(6.66016032936793,-9.43268772516334,-60.));
#6385=CARTESIAN_POINT('Origin',(-16.3378943919142,-11.5357360770199,-60.));
#6386=CARTESIAN_POINT('',(-4.83886703127313,-10.4842119010916,-60.));
#6387=CARTESIAN_POINT('',(6.66016032936793,-9.43268772516334,-60.));
#6388=CARTESIAN_POINT('',(-4.83886703127313,-10.4842119010916,-60.));
#6389=CARTESIAN_POINT('Origin',(-16.3378943919142,-11.5357360770199,-60.));
#6390=CARTESIAN_POINT('',(-11.4990273606411,-1.0515241759283,-60.));
#6391=CARTESIAN_POINT('',(-4.83886703127313,-10.4842119010916,-60.));
#6392=CARTESIAN_POINT('',(-11.4990273606411,-1.0515241759283,-60.));
#6393=CARTESIAN_POINT('Origin',(6.66016032936793,-9.43268772516334,-68.));
#6394=CARTESIAN_POINT('',(-4.83886703127313,-10.4842119010916,-68.));
#6395=CARTESIAN_POINT('',(6.66016032936793,-9.43268772516334,-68.));
#6396=CARTESIAN_POINT('Origin',(-4.83886703127313,-10.4842119010916,-68.));
#6397=CARTESIAN_POINT('',(-11.4990273606411,-1.0515241759283,-68.));
#6398=CARTESIAN_POINT('Origin',(-11.4990273606411,-1.0515241759283,-68.));
#6399=CARTESIAN_POINT('',(-6.66016032936793,9.43268772516333,-68.));
#6400=CARTESIAN_POINT('Origin',(-6.66016032936793,9.43268772516333,-68.));
#6401=CARTESIAN_POINT('',(4.83886703127313,10.4842119010916,-68.));
#6402=CARTESIAN_POINT('Origin',(4.83886703127313,10.4842119010916,-68.));
#6403=CARTESIAN_POINT('',(11.4990273606411,1.05152417592829,-68.));
#6404=CARTESIAN_POINT('Origin',(11.4990273606411,1.05152417592829,-68.));
#6405=CARTESIAN_POINT('Origin',(0.,5.,-170.));
#6406=CARTESIAN_POINT('Origin',(0.,6.,-148.));
#6407=CARTESIAN_POINT('',(0.,0.,0.));
#6408=CARTESIAN_POINT('Origin',(14.,10.,0.));
#6409=CARTESIAN_POINT('',(14.,9.5,-1.4142135623731));
#6410=CARTESIAN_POINT('',(14.,10.5,-1.4142135623731));
#6411=CARTESIAN_POINT('Origin',(14.,10.,0.));
#6412=CARTESIAN_POINT('',(-14.,9.5,-1.4142135623731));
#6413=CARTESIAN_POINT('',(14.,9.5,-1.4142135623731));
#6414=CARTESIAN_POINT('',(-14.,10.5,-1.4142135623731));
#6415=CARTESIAN_POINT('Origin',(-14.,10.,0.));
#6416=CARTESIAN_POINT('',(14.,10.5,-1.4142135623731));
#6417=CARTESIAN_POINT('Origin',(14.,10.,0.));
#6418=CARTESIAN_POINT('',(14.,10.5,-2.44948974278318));
#6419=CARTESIAN_POINT('',(14.,9.5,-2.44948974278318));
#6420=CARTESIAN_POINT('Origin',(14.,10.,0.));
#6421=CARTESIAN_POINT('',(13.5,10.5,-2.44948974278318));
#6422=CARTESIAN_POINT('',(14.,10.5,-2.44948974278318));
#6423=CARTESIAN_POINT('',(13.5,9.5,-2.44948974278318));
#6424=CARTESIAN_POINT('Origin',(13.5,10.,0.));
#6425=CARTESIAN_POINT('',(14.,9.5,-2.44948974278318));
#6426=CARTESIAN_POINT('Origin',(14.,10.,0.));
#6427=CARTESIAN_POINT('',(-13.5,10.5,-2.44948974278318));
#6428=CARTESIAN_POINT('',(-13.5,9.5,-2.44948974278318));
#6429=CARTESIAN_POINT('Origin',(-13.5,10.,0.));
#6430=CARTESIAN_POINT('',(-14.,10.5,-2.44948974278318));
#6431=CARTESIAN_POINT('',(14.,10.5,-2.44948974278318));
#6432=CARTESIAN_POINT('',(-14.,9.5,-2.44948974278318));
#6433=CARTESIAN_POINT('Origin',(-14.,10.,0.));
#6434=CARTESIAN_POINT('',(14.,9.5,-2.44948974278318));
#6435=CARTESIAN_POINT('Origin',(0.,0.,10.1));
#6436=CARTESIAN_POINT('',(6.,-7.34788079488412E-16,10.1));
#6437=CARTESIAN_POINT('Origin',(0.,0.,10.1));
#6438=CARTESIAN_POINT('',(6.,-7.34788079488412E-16,-10.1));
#6439=CARTESIAN_POINT('',(6.,-7.34788079488412E-16,10.1));
#6440=CARTESIAN_POINT('Origin',(0.,0.,-10.1));
#6441=CARTESIAN_POINT('Origin',(0.,0.,10.1));
#6442=CARTESIAN_POINT('',(10.,-1.22464679914735E-15,10.));
#6443=CARTESIAN_POINT('Origin',(0.,0.,10.));
#6444=CARTESIAN_POINT('',(10.,-1.22464679914735E-15,10.1));
#6445=CARTESIAN_POINT('',(10.,-1.22464679914735E-15,10.1));
#6446=CARTESIAN_POINT('Origin',(0.,0.,10.1));
#6447=CARTESIAN_POINT('Origin',(0.,0.,10.1));
#6448=CARTESIAN_POINT('',(10.,-1.22464679914735E-15,-10.1));
#6449=CARTESIAN_POINT('Origin',(0.,0.,-10.1));
#6450=CARTESIAN_POINT('',(10.,-1.22464679914735E-15,-10.));
#6451=CARTESIAN_POINT('',(10.,-1.22464679914735E-15,10.1));
#6452=CARTESIAN_POINT('Origin',(0.,0.,-10.));
#6453=CARTESIAN_POINT('Origin',(7.75,28.,0.));
#6454=CARTESIAN_POINT('',(13.,28.,-5.));
#6455=CARTESIAN_POINT('Origin',(13.,28.,0.));
#6456=CARTESIAN_POINT('Origin',(13.,28.,0.));
#6457=CARTESIAN_POINT('',(9.,28.,-5.));
#6458=CARTESIAN_POINT('Origin',(9.,28.,0.));
#6459=CARTESIAN_POINT('',(13.,28.,-5.));
#6460=CARTESIAN_POINT('Origin',(13.,28.,0.));
#6461=CARTESIAN_POINT('',(-5.,28.,-5.));
#6462=CARTESIAN_POINT('Origin',(-5.,28.,0.));
#6463=CARTESIAN_POINT('',(5.,28.,-5.));
#6464=CARTESIAN_POINT('',(13.,28.,-5.));
#6465=CARTESIAN_POINT('Origin',(5.,28.,0.));
#6466=CARTESIAN_POINT('Origin',(13.,28.,0.));
#6467=CARTESIAN_POINT('',(-13.,28.,-5.));
#6468=CARTESIAN_POINT('Origin',(-13.,28.,0.));
#6469=CARTESIAN_POINT('',(-9.,28.,-5.));
#6470=CARTESIAN_POINT('',(13.,28.,-5.));
#6471=CARTESIAN_POINT('Origin',(-9.,28.,0.));
#6472=CARTESIAN_POINT('Origin',(-7.75,28.,0.));
#6473=CARTESIAN_POINT('Origin',(13.,-28.,0.));
#6474=CARTESIAN_POINT('',(-13.,-28.,-5.));
#6475=CARTESIAN_POINT('Origin',(-13.,-28.,0.));
#6476=CARTESIAN_POINT('',(-9.,-28.,-5.));
#6477=CARTESIAN_POINT('',(13.,-28.,-5.));
#6478=CARTESIAN_POINT('Origin',(-9.,-28.,0.));
#6479=CARTESIAN_POINT('Origin',(13.,-28.,0.));
#6480=CARTESIAN_POINT('',(-5.,-28.,-5.));
#6481=CARTESIAN_POINT('Origin',(-5.,-28.,0.));
#6482=CARTESIAN_POINT('',(5.,-28.,-5.));
#6483=CARTESIAN_POINT('',(13.,-28.,-5.));
#6484=CARTESIAN_POINT('Origin',(5.,-28.,0.));
#6485=CARTESIAN_POINT('Origin',(13.,-28.,0.));
#6486=CARTESIAN_POINT('',(9.,-28.,-5.));
#6487=CARTESIAN_POINT('Origin',(9.,-28.,0.));
#6488=CARTESIAN_POINT('',(13.,-28.,-5.));
#6489=CARTESIAN_POINT('',(13.,-28.,-5.));
#6490=CARTESIAN_POINT('Origin',(13.,-28.,0.));
#6491=CARTESIAN_POINT('Origin',(-15.,10.,0.));
#6492=CARTESIAN_POINT('Origin',(-13.5,10.,0.));
#6493=CARTESIAN_POINT('',(-15.,9.5,-2.44948974278318));
#6494=CARTESIAN_POINT('Origin',(13.5,10.,0.));
#6495=CARTESIAN_POINT('',(-15.,10.5,-2.44948974278318));
#6496=CARTESIAN_POINT('Origin',(-9.,17.,10.));
#6497=CARTESIAN_POINT('',(9.,17.,10.));
#6498=CARTESIAN_POINT('',(9.,28.,10.));
#6499=CARTESIAN_POINT('',(9.,17.,10.));
#6500=CARTESIAN_POINT('',(5.,28.,10.));
#6501=CARTESIAN_POINT('',(13.5,28.,10.));
#6502=CARTESIAN_POINT('',(5.,17.,10.));
#6503=CARTESIAN_POINT('',(5.,38.,10.));
#6504=CARTESIAN_POINT('',(-5.,17.,10.));
#6505=CARTESIAN_POINT('',(-5.,17.,10.));
#6506=CARTESIAN_POINT('',(-5.,28.,10.));
#6507=CARTESIAN_POINT('',(-5.,38.,10.));
#6508=CARTESIAN_POINT('',(-9.,28.,10.));
#6509=CARTESIAN_POINT('',(13.5,28.,10.));
#6510=CARTESIAN_POINT('',(-9.,17.,10.));
#6511=CARTESIAN_POINT('',(-9.,17.,10.));
#6512=CARTESIAN_POINT('',(-13.5,17.,10.));
#6513=CARTESIAN_POINT('',(-13.5,17.,10.));
#6514=CARTESIAN_POINT('',(-13.5,-17.,10.));
#6515=CARTESIAN_POINT('',(-13.5,-17.,10.));
#6516=CARTESIAN_POINT('',(-9.,-17.,10.));
#6517=CARTESIAN_POINT('',(-13.5,-17.,10.));
#6518=CARTESIAN_POINT('',(-9.,-28.,10.));
#6519=CARTESIAN_POINT('',(-9.,-17.,10.));
#6520=CARTESIAN_POINT('',(-5.,-28.,10.));
#6521=CARTESIAN_POINT('',(13.5,-28.,10.));
#6522=CARTESIAN_POINT('',(-5.,-17.,10.));
#6523=CARTESIAN_POINT('',(-5.,-38.,10.));
#6524=CARTESIAN_POINT('',(5.,-17.,10.));
#6525=CARTESIAN_POINT('',(-5.,-17.,10.));
#6526=CARTESIAN_POINT('',(5.,-28.,10.));
#6527=CARTESIAN_POINT('',(5.,-38.,10.));
#6528=CARTESIAN_POINT('',(9.,-28.,10.));
#6529=CARTESIAN_POINT('',(13.5,-28.,10.));
#6530=CARTESIAN_POINT('',(9.,-17.,10.));
#6531=CARTESIAN_POINT('',(9.,-17.,10.));
#6532=CARTESIAN_POINT('',(13.5,-17.,10.));
#6533=CARTESIAN_POINT('',(13.5,-17.,10.));
#6534=CARTESIAN_POINT('',(13.5,17.,10.));
#6535=CARTESIAN_POINT('',(13.5,-17.,10.));
#6536=CARTESIAN_POINT('',(13.5,17.,10.));
#6537=CARTESIAN_POINT('Origin',(-9.,17.,-10.));
#6538=CARTESIAN_POINT('',(9.,28.,-10.));
#6539=CARTESIAN_POINT('',(5.,28.,-10.));
#6540=CARTESIAN_POINT('',(13.5,28.,-10.));
#6541=CARTESIAN_POINT('',(9.,17.,-10.));
#6542=CARTESIAN_POINT('',(9.,17.,-10.));
#6543=CARTESIAN_POINT('',(13.5,17.,-10.));
#6544=CARTESIAN_POINT('',(13.5,17.,-10.));
#6545=CARTESIAN_POINT('',(13.5,-17.,-10.));
#6546=CARTESIAN_POINT('',(13.5,-17.,-10.));
#6547=CARTESIAN_POINT('',(9.,-17.,-10.));
#6548=CARTESIAN_POINT('',(13.5,-17.,-10.));
#6549=CARTESIAN_POINT('',(9.,-28.,-10.));
#6550=CARTESIAN_POINT('',(9.,-17.,-10.));
#6551=CARTESIAN_POINT('',(5.,-28.,-10.));
#6552=CARTESIAN_POINT('',(13.5,-28.,-10.));
#6553=CARTESIAN_POINT('',(5.,-17.,-10.));
#6554=CARTESIAN_POINT('',(5.,-38.,-10.));
#6555=CARTESIAN_POINT('',(-5.,-17.,-10.));
#6556=CARTESIAN_POINT('',(-5.,-17.,-10.));
#6557=CARTESIAN_POINT('',(-5.,-28.,-10.));
#6558=CARTESIAN_POINT('',(-5.,-38.,-10.));
#6559=CARTESIAN_POINT('',(-9.,-28.,-10.));
#6560=CARTESIAN_POINT('',(13.5,-28.,-10.));
#6561=CARTESIAN_POINT('',(-9.,-17.,-10.));
#6562=CARTESIAN_POINT('',(-9.,-17.,-10.));
#6563=CARTESIAN_POINT('',(-13.5,-17.,-10.));
#6564=CARTESIAN_POINT('',(-13.5,-17.,-10.));
#6565=CARTESIAN_POINT('',(-13.5,17.,-10.));
#6566=CARTESIAN_POINT('',(-13.5,-17.,-10.));
#6567=CARTESIAN_POINT('',(-9.,17.,-10.));
#6568=CARTESIAN_POINT('',(-13.5,17.,-10.));
#6569=CARTESIAN_POINT('',(-9.,28.,-10.));
#6570=CARTESIAN_POINT('',(-9.,17.,-10.));
#6571=CARTESIAN_POINT('',(-5.,28.,-10.));
#6572=CARTESIAN_POINT('',(13.5,28.,-10.));
#6573=CARTESIAN_POINT('',(-5.,17.,-10.));
#6574=CARTESIAN_POINT('',(-5.,38.,-10.));
#6575=CARTESIAN_POINT('',(5.,17.,-10.));
#6576=CARTESIAN_POINT('',(-5.,17.,-10.));
#6577=CARTESIAN_POINT('',(5.,38.,-10.));
#6578=CARTESIAN_POINT('Origin',(-9.,-17.,10.));
#6579=CARTESIAN_POINT('Origin',(-9.,-28.,0.));
#6580=CARTESIAN_POINT('',(-9.,-17.,10.));
#6581=CARTESIAN_POINT('Origin',(-5.,-38.,10.));
#6582=CARTESIAN_POINT('Origin',(-5.,-28.,0.));
#6583=CARTESIAN_POINT('',(-5.,-17.,10.));
#6584=CARTESIAN_POINT('Origin',(5.,-38.,10.));
#6585=CARTESIAN_POINT('Origin',(5.,-28.,0.));
#6586=CARTESIAN_POINT('',(5.,-17.,10.));
#6587=CARTESIAN_POINT('Origin',(9.,-17.,10.));
#6588=CARTESIAN_POINT('Origin',(9.,-28.,0.));
#6589=CARTESIAN_POINT('',(9.,-17.,10.));
#6590=CARTESIAN_POINT('Origin',(9.,17.,10.));
#6591=CARTESIAN_POINT('Origin',(9.,28.,0.));
#6592=CARTESIAN_POINT('',(9.,17.,10.));
#6593=CARTESIAN_POINT('Origin',(5.,38.,10.));
#6594=CARTESIAN_POINT('Origin',(5.,28.,0.));
#6595=CARTESIAN_POINT('',(5.,17.,10.));
#6596=CARTESIAN_POINT('Origin',(-5.,38.,10.));
#6597=CARTESIAN_POINT('Origin',(-5.,28.,0.));
#6598=CARTESIAN_POINT('',(-5.,17.,10.));
#6599=CARTESIAN_POINT('Origin',(-9.,17.,10.));
#6600=CARTESIAN_POINT('Origin',(-9.,28.,0.));
#6601=CARTESIAN_POINT('',(-9.,17.,10.));
#6602=CARTESIAN_POINT('Origin',(-13.5,17.,10.));
#6603=CARTESIAN_POINT('',(-13.5,17.,10.));
#6604=CARTESIAN_POINT('Origin',(-13.5,-17.,10.));
#6605=CARTESIAN_POINT('',(-13.5,-17.,10.));
#6606=CARTESIAN_POINT('Origin',(-13.5,-17.,10.));
#6607=CARTESIAN_POINT('Origin',(-5.,-17.,10.));
#6608=CARTESIAN_POINT('Origin',(13.5,-17.,10.));
#6609=CARTESIAN_POINT('',(13.5,-17.,10.));
#6610=CARTESIAN_POINT('Origin',(13.5,-17.,10.));
#6611=CARTESIAN_POINT('',(13.5,17.,10.));
#6612=CARTESIAN_POINT('Origin',(13.5,17.,10.));
#6613=CARTESIAN_POINT('Origin',(-5.,17.,10.));
#6614=CARTESIAN_POINT('Origin',(13.5,28.,0.));
#6615=CARTESIAN_POINT('Origin',(13.5,28.,0.));
#6616=CARTESIAN_POINT('Origin',(13.5,-28.,0.));
#6617=CARTESIAN_POINT('Origin',(13.5,-28.,0.));
#6618=CARTESIAN_POINT('Origin',(13.,-28.,0.));
#6619=CARTESIAN_POINT('Origin',(-13.,-28.,0.));
#6620=CARTESIAN_POINT('Origin',(0.,0.,10.1));
#6621=CARTESIAN_POINT('Origin',(0.,0.,-10.1));
#6622=CARTESIAN_POINT('Origin',(14.,10.5,-1.4142135623731));
#6623=CARTESIAN_POINT('',(-14.,10.5,-1.4142135623731));
#6624=CARTESIAN_POINT('',(14.,10.5,-1.4142135623731));
#6625=CARTESIAN_POINT('Origin',(14.,9.5,-1.4142135623731));
#6626=CARTESIAN_POINT('',(-14.,9.5,-1.4142135623731));
#6627=CARTESIAN_POINT('',(14.,9.5,-1.4142135623731));
#6628=CARTESIAN_POINT('Origin',(14.,10.,0.));
#6629=CARTESIAN_POINT('Origin',(-14.,10.,0.));
#6630=CARTESIAN_POINT('',(0.,0.,0.));
#6631=CARTESIAN_POINT('Origin',(24.,0.,2.));
#6632=CARTESIAN_POINT('',(29.,-6.12323399573677E-16,2.));
#6633=CARTESIAN_POINT('Origin',(24.,0.,2.));
#6634=CARTESIAN_POINT('',(29.,-6.12323399573677E-16,-2.));
#6635=CARTESIAN_POINT('',(29.,-6.12323399573677E-16,2.));
#6636=CARTESIAN_POINT('Origin',(24.,0.,-2.));
#6637=CARTESIAN_POINT('Origin',(0.,0.,2.));
#6638=CARTESIAN_POINT('',(5.,-6.12323399573677E-16,2.));
#6639=CARTESIAN_POINT('Origin',(0.,0.,2.));
#6640=CARTESIAN_POINT('',(5.,-6.12323399573677E-16,-2.));
#6641=CARTESIAN_POINT('',(5.,-6.12323399573677E-16,2.));
#6642=CARTESIAN_POINT('Origin',(0.,0.,-2.));
#6643=CARTESIAN_POINT('Origin',(0.,0.,2.));
#6644=CARTESIAN_POINT('',(0.,10.,2.));
#6645=CARTESIAN_POINT('',(1.22460635382238E-15,-10.,2.));
#6646=CARTESIAN_POINT('Origin',(0.,0.,2.));
#6647=CARTESIAN_POINT('',(0.,10.,-2.));
#6648=CARTESIAN_POINT('',(0.,10.,2.));
#6649=CARTESIAN_POINT('',(1.22460635382238E-15,-10.,-2.));
#6650=CARTESIAN_POINT('Origin',(0.,0.,-2.));
#6651=CARTESIAN_POINT('',(1.22460635382238E-15,-10.,2.));
#6652=CARTESIAN_POINT('Origin',(0.,0.,2.));
#6653=CARTESIAN_POINT('',(24.,-10.,2.));
#6654=CARTESIAN_POINT('',(24.,-10.,2.));
#6655=CARTESIAN_POINT('',(24.,10.,2.));
#6656=CARTESIAN_POINT('Origin',(24.,0.,2.));
#6657=CARTESIAN_POINT('',(0.,10.,2.));
#6658=CARTESIAN_POINT('Origin',(0.,0.,-2.));
#6659=CARTESIAN_POINT('',(24.,10.,-2.));
#6660=CARTESIAN_POINT('',(0.,10.,-2.));
#6661=CARTESIAN_POINT('',(24.,-10.,-2.));
#6662=CARTESIAN_POINT('Origin',(24.,0.,-2.));
#6663=CARTESIAN_POINT('',(24.,-10.,-2.));
#6664=CARTESIAN_POINT('Origin',(24.,-10.,2.));
#6665=CARTESIAN_POINT('',(24.,-10.,2.));
#6666=CARTESIAN_POINT('Origin',(24.,0.,2.));
#6667=CARTESIAN_POINT('',(24.,10.,2.));
#6668=CARTESIAN_POINT('Origin',(0.,10.,2.));
#6669=CARTESIAN_POINT('',(0.,0.,0.));
#6670=CARTESIAN_POINT('Origin',(0.,0.,25.));
#6671=CARTESIAN_POINT('',(5.,-6.12323399573676E-16,24.));
#6672=CARTESIAN_POINT('Origin',(0.,0.,24.));
#6673=CARTESIAN_POINT('',(3.99999999999998,-4.89858719658939E-16,25.));
#6674=CARTESIAN_POINT('',(3.99999999999998,-4.89858719658939E-16,25.));
#6675=CARTESIAN_POINT('Origin',(0.,0.,25.));
#6676=CARTESIAN_POINT('Origin',(-10.352761804101,-38.6370330515627,13.));
#6677=CARTESIAN_POINT('',(-5.35276180410099,-38.6370330515627,12.));
#6678=CARTESIAN_POINT('Origin',(-10.352761804101,-38.6370330515627,12.));
#6679=CARTESIAN_POINT('',(-6.35276180410101,-38.6370330515627,13.));
#6680=CARTESIAN_POINT('',(-6.35276180410101,-38.6370330515627,13.));
#6681=CARTESIAN_POINT('Origin',(-10.352761804101,-38.6370330515627,13.));
#6682=CARTESIAN_POINT('Origin',(0.,0.,-24.));
#6683=CARTESIAN_POINT('',(5.,6.12323399573676E-16,-24.));
#6684=CARTESIAN_POINT('',(-5.,-6.12323399573676E-16,-24.));
#6685=CARTESIAN_POINT('Origin',(0.,0.,-24.));
#6686=CARTESIAN_POINT('Origin',(0.,0.,-24.));
#6687=CARTESIAN_POINT('',(-3.99999999999999,-4.8985871965894E-16,-25.));
#6688=CARTESIAN_POINT('',(-5.,-6.12323399573676E-16,-24.));
#6689=CARTESIAN_POINT('Origin',(0.,0.,-25.));
#6690=CARTESIAN_POINT('Origin',(-10.352761804101,-38.6370330515627,-12.));
#6691=CARTESIAN_POINT('',(-5.35276180410099,-38.6370330515627,-12.));
#6692=CARTESIAN_POINT('',(-15.352761804101,-38.6370330515627,-12.));
#6693=CARTESIAN_POINT('Origin',(-10.352761804101,-38.6370330515627,-12.));
#6694=CARTESIAN_POINT('Origin',(-10.352761804101,-38.6370330515627,-12.));
#6695=CARTESIAN_POINT('',(-14.352761804101,-38.6370330515627,-13.));
#6696=CARTESIAN_POINT('',(-15.352761804101,-38.6370330515627,-12.));
#6697=CARTESIAN_POINT('Origin',(-10.352761804101,-38.6370330515627,-13.));
#6698=CARTESIAN_POINT('Origin',(-10.352761804101,-38.6370330515627,13.));
#6699=CARTESIAN_POINT('',(-5.35276180410099,-38.6370330515627,10.));
#6700=CARTESIAN_POINT('Origin',(-10.352761804101,-38.6370330515627,10.));
#6701=CARTESIAN_POINT('',(-5.35276180410099,-38.6370330515627,13.));
#6702=CARTESIAN_POINT('Origin',(-10.352761804101,-38.6370330515627,13.));
#6703=CARTESIAN_POINT('',(-5.35276180410099,-38.6370330515627,-10.));
#6704=CARTESIAN_POINT('',(-5.35276180410099,-38.6370330515627,13.));
#6705=CARTESIAN_POINT('Origin',(-10.352761804101,-38.6370330515627,-10.));
#6706=CARTESIAN_POINT('Origin',(-10.352761804101,-38.6370330515627,13.));
#6707=CARTESIAN_POINT('',(-5.35276180410099,-38.6370330515627,-5.));
#6708=CARTESIAN_POINT('Origin',(-10.352761804101,-38.6370330515627,-5.));
#6709=CARTESIAN_POINT('',(-5.35276180410099,-38.6370330515627,5.));
#6710=CARTESIAN_POINT('',(-5.35276180410099,-38.6370330515627,13.));
#6711=CARTESIAN_POINT('Origin',(-10.352761804101,-38.6370330515627,5.));
#6712=CARTESIAN_POINT('Origin',(0.,0.,25.));
#6713=CARTESIAN_POINT('',(5.,-6.12323399573676E-16,15.));
#6714=CARTESIAN_POINT('Origin',(0.,0.,15.));
#6715=CARTESIAN_POINT('',(5.,-6.12323399573676E-16,25.));
#6716=CARTESIAN_POINT('Origin',(0.,0.,25.));
#6717=CARTESIAN_POINT('',(5.,-6.12323399573676E-16,-15.));
#6718=CARTESIAN_POINT('',(5.,-6.12323399573676E-16,25.));
#6719=CARTESIAN_POINT('Origin',(0.,0.,-15.));
#6720=CARTESIAN_POINT('Origin',(-10.352761804101,-38.6370330515627,-8.));
#6721=CARTESIAN_POINT('',(-20.0120200669917,-36.0488426005374,-8.));
#6722=CARTESIAN_POINT('',(-0.693503541210314,-41.2252235025879,-8.));
#6723=CARTESIAN_POINT('Origin',(-10.352761804101,-38.6370330515627,-8.));
#6724=CARTESIAN_POINT('',(-18.0801684144135,-36.5664806907425,-10.));
#6725=CARTESIAN_POINT('Origin',(-18.0801684144135,-36.5664806907425,-8.));
#6726=CARTESIAN_POINT('',(-2.62535519378845,-40.7075854123829,-10.));
#6727=CARTESIAN_POINT('Origin',(-10.352761804101,-38.6370330515627,-10.));
#6728=CARTESIAN_POINT('Origin',(-2.62535519378845,-40.7075854123829,-8.));
#6729=CARTESIAN_POINT('Origin',(0.,0.,12.));
#6730=CARTESIAN_POINT('',(-8.36862877099655,-5.47412572866653,12.));
#6731=CARTESIAN_POINT('',(10.,-1.22464679914735E-15,12.));
#6732=CARTESIAN_POINT('Origin',(0.,0.,12.));
#6733=CARTESIAN_POINT('',(-10.0423545251959,-6.56895087439983,10.));
#6734=CARTESIAN_POINT('Origin',(-10.0423545251959,-6.56895087439983,12.));
#6735=CARTESIAN_POINT('',(8.94427190999916,8.,10.));
#6736=CARTESIAN_POINT('Origin',(0.,0.,10.));
#6737=CARTESIAN_POINT('',(7.4535599249993,6.66666666666667,12.));
#6738=CARTESIAN_POINT('Origin',(8.94427190999916,8.,12.));
#6739=CARTESIAN_POINT('Origin',(0.,0.,12.));
#6740=CARTESIAN_POINT('Origin',(80.,0.,28.));
#6741=CARTESIAN_POINT('',(80.,10.,28.));
#6742=CARTESIAN_POINT('',(80.,-10.,28.));
#6743=CARTESIAN_POINT('Origin',(80.,0.,28.));
#6744=CARTESIAN_POINT('',(80.,8.,30.));
#6745=CARTESIAN_POINT('Origin',(80.,8.,28.));
#6746=CARTESIAN_POINT('',(80.,-8.,30.));
#6747=CARTESIAN_POINT('Origin',(80.,0.,30.));
#6748=CARTESIAN_POINT('Origin',(80.,-8.,28.));
#6749=CARTESIAN_POINT('Origin',(80.,0.,-30.));
#6750=CARTESIAN_POINT('',(85.,6.12323399573677E-16,-30.));
#6751=CARTESIAN_POINT('Origin',(80.,0.,-30.));
#6752=CARTESIAN_POINT('',(85.,6.12323399573677E-16,-22.));
#6753=CARTESIAN_POINT('',(85.,6.12323399573677E-16,-30.));
#6754=CARTESIAN_POINT('Origin',(80.,0.,-22.));
#6755=CARTESIAN_POINT('Origin',(-10.352761804101,-38.6370330515627,-30.));
#6756=CARTESIAN_POINT('',(-0.693503541210314,-41.2252235025879,-5.));
#6757=CARTESIAN_POINT('',(-0.693503541210314,-41.2252235025879,-30.));
#6758=CARTESIAN_POINT('',(-20.0120200669917,-36.0488426005374,-5.));
#6759=CARTESIAN_POINT('Origin',(-10.352761804101,-38.6370330515627,-5.));
#6760=CARTESIAN_POINT('',(-20.0120200669917,-36.0488426005374,-30.));
#6761=CARTESIAN_POINT('Origin',(80.,0.,30.));
#6762=CARTESIAN_POINT('',(85.,-6.12323399573677E-16,30.));
#6763=CARTESIAN_POINT('Origin',(80.,0.,30.));
#6764=CARTESIAN_POINT('',(85.,-6.12323399573677E-16,22.));
#6765=CARTESIAN_POINT('',(85.,-6.12323399573677E-16,30.));
#6766=CARTESIAN_POINT('Origin',(80.,0.,22.));
#6767=CARTESIAN_POINT('Origin',(-10.352761804101,-38.6370330515627,30.));
#6768=CARTESIAN_POINT('',(-0.693503541210314,-41.2252235025879,8.));
#6769=CARTESIAN_POINT('',(-20.0120200669917,-36.0488426005374,8.));
#6770=CARTESIAN_POINT('Origin',(-10.352761804101,-38.6370330515627,8.));
#6771=CARTESIAN_POINT('',(-20.0120200669917,-36.0488426005374,5.));
#6772=CARTESIAN_POINT('',(-20.0120200669917,-36.0488426005374,30.));
#6773=CARTESIAN_POINT('',(-0.693503541210314,-41.2252235025879,5.));
#6774=CARTESIAN_POINT('Origin',(-10.352761804101,-38.6370330515627,5.));
#6775=CARTESIAN_POINT('',(-0.693503541210314,-41.2252235025879,30.));
#6776=CARTESIAN_POINT('Origin',(0.,0.,30.));
#6777=CARTESIAN_POINT('',(10.,-1.22464679914735E-15,-15.));
#6778=CARTESIAN_POINT('Origin',(0.,0.,-15.));
#6779=CARTESIAN_POINT('',(10.,-1.22464679914735E-15,-12.));
#6780=CARTESIAN_POINT('',(10.,-1.22464679914735E-15,30.));
#6781=CARTESIAN_POINT('',(-8.36862877099655,-5.47412572866653,-12.));
#6782=CARTESIAN_POINT('Origin',(0.,0.,-12.));
#6783=CARTESIAN_POINT('',(-10.0001237867953,1.97103394976209E-9,-9.76179717313037));
#6784=CARTESIAN_POINT('Ctrl Pts',(-8.36862877099655,-5.47412572866653,-12.));
#6785=CARTESIAN_POINT('Ctrl Pts',(-8.45441677353284,-5.3429763941761,-11.999999997427));
#6786=CARTESIAN_POINT('Ctrl Pts',(-8.53638588592189,-5.21097527038014,-11.9927750050672));
#6787=CARTESIAN_POINT('Ctrl Pts',(-8.61474990666338,-5.07804162738316,-11.9792446203911));
#6788=CARTESIAN_POINT('Ctrl Pts',(-8.69764757311686,-4.93741728609315,-11.9649314533886));
#6789=CARTESIAN_POINT('Ctrl Pts',(-8.7765110195439,-4.79574947320889,-11.9435619214423));
#6790=CARTESIAN_POINT('Ctrl Pts',(-8.85157147514725,-4.65293688559633,-11.9161702848848));
#6791=CARTESIAN_POINT('Ctrl Pts',(-8.88099655546167,-4.59695172234851,-11.9054322591271));
#6792=CARTESIAN_POINT('Ctrl Pts',(-8.90983696513968,-4.54079056665035,-11.8937682266929));
#6793=CARTESIAN_POINT('Ctrl Pts',(-8.93810575967581,-4.4844470594322,-11.8812385781177));
#6794=CARTESIAN_POINT('Ctrl Pts',(-9.00060480640978,-4.35987805857574,-11.8535369691632));
#6795=CARTESIAN_POINT('Ctrl Pts',(-9.06035407011131,-4.23417994539579,-11.8214303185381));
#6796=CARTESIAN_POINT('Ctrl Pts',(-9.11723772204825,-4.107888608141,-11.7855218310165));
#6797=CARTESIAN_POINT('Ctrl Pts',(-9.17291702662629,-3.9842711259095,-11.7503736022096));
#6798=CARTESIAN_POINT('Ctrl Pts',(-9.22565175869234,-3.86052975248589,-11.7117034479191));
#6799=CARTESIAN_POINT('Ctrl Pts',(-9.27540566403723,-3.73710738033695,-11.6701121216955));
#6800=CARTESIAN_POINT('Ctrl Pts',(-9.31297518633027,-3.64391028294799,-11.6387062200497));
#6801=CARTESIAN_POINT('Ctrl Pts',(-9.34884483253428,-3.55089436934357,-11.6056335296996));
#6802=CARTESIAN_POINT('Ctrl Pts',(-9.3829931498531,-3.45824226410632,-11.5711359915397));
#6803=CARTESIAN_POINT('Ctrl Pts',(-9.4344758472812,-3.31855806662537,-11.5191268016721));
#6804=CARTESIAN_POINT('Ctrl Pts',(-9.48228811673317,-3.17928629062166,-11.4637999274883));
#6805=CARTESIAN_POINT('Ctrl Pts',(-9.52668028722712,-3.04019414324163,-11.4054943378528));
#6806=CARTESIAN_POINT('Ctrl Pts',(-9.56112163353964,-2.93228050072395,-11.3602583653323));
#6807=CARTESIAN_POINT('Ctrl Pts',(-9.5935035091139,-2.8244750314983,-11.3132284064526));
#6808=CARTESIAN_POINT('Ctrl Pts',(-9.62392825897893,-2.71666946271822,-11.2645470181033));
#6809=CARTESIAN_POINT('Ctrl Pts',(-9.65106802401281,-2.62050374832403,-11.2211217985967));
#6810=CARTESIAN_POINT('Ctrl Pts',(-9.67662805956223,-2.52441492191825,-11.1764028555152));
#6811=CARTESIAN_POINT('Ctrl Pts',(-9.70066935863215,-2.42837682308185,-11.1305171637202));
#6812=CARTESIAN_POINT('Ctrl Pts',(-9.73425070221459,-2.29422898087712,-11.0664231571024));
#6813=CARTESIAN_POINT('Ctrl Pts',(-9.76488031347849,-2.16005590238908,-10.9999667510052));
#6814=CARTESIAN_POINT('Ctrl Pts',(-9.79262273697897,-2.02595889184267,-10.9314471311979));
#6815=CARTESIAN_POINT('Ctrl Pts',(-9.81788538848297,-1.90384821736955,-10.8690521758203));
#6816=CARTESIAN_POINT('Ctrl Pts',(-9.84075817492368,-1.78176050965276,-10.8049283493925));
#6817=CARTESIAN_POINT('Ctrl Pts',(-9.86124220206778,-1.66008483923076,-10.7394558128057));
#6818=CARTESIAN_POINT('Ctrl Pts',(-9.87618462610704,-1.57132643982444,-10.6916957508939));
#6819=CARTESIAN_POINT('Ctrl Pts',(-9.8898569179316,-1.48278733165533,-10.6432187826923));
#6820=CARTESIAN_POINT('Ctrl Pts',(-9.90227459651842,-1.39461744436331,-10.5941810273421));
#6821=CARTESIAN_POINT('Ctrl Pts',(-9.90491108546458,-1.37589744516181,-10.5837694597515));
#6822=CARTESIAN_POINT('Ctrl Pts',(-9.90749042320112,-1.35720601089956,-10.5733402505487));
#6823=CARTESIAN_POINT('Ctrl Pts',(-9.91001294263523,-1.33854404163214,-10.5628944871018));
#6824=CARTESIAN_POINT('Ctrl Pts',(-9.93626127877299,-1.1443549956723,-10.4542000182056));
#6825=CARTESIAN_POINT('Ctrl Pts',(-9.95656708456508,-0.951820837724888,
-10.3428183419215));
#6826=CARTESIAN_POINT('Ctrl Pts',(-9.97120936406249,-0.760674650770803,
-10.2291898572203));
#6827=CARTESIAN_POINT('Ctrl Pts',(-9.98607735096438,-0.566581988867939,
-10.1138098153001));
#6828=CARTESIAN_POINT('Ctrl Pts',(-9.99510564348261,-0.373919899057051,
-9.99611300520595));
#6829=CARTESIAN_POINT('Ctrl Pts',(-9.99856425937658,-0.182425776511984,
-9.876514630881));
#6830=CARTESIAN_POINT('Ctrl Pts',(-9.99966462607587,-0.121501475573082,
-9.83846412963148));
#6831=CARTESIAN_POINT('Ctrl Pts',(-10.0002010743077,-0.0606955535016998,
-9.80022081609969));
#6832=CARTESIAN_POINT('Ctrl Pts',(-10.0001819091909,-1.39135034132474E-8,
-9.76179714435925));
#6833=CARTESIAN_POINT('',(-9.65925826289068,2.58819045102525,-8.));
#6834=CARTESIAN_POINT('Ctrl Pts',(-10.,3.58012980029344E-8,-9.76179723440599));
#6835=CARTESIAN_POINT('Ctrl Pts',(-10.,0.441544717876623,-9.48226950053063));
#6836=CARTESIAN_POINT('Ctrl Pts',(-9.97097024786624,0.87720718112473,-9.19317827898892));
#6837=CARTESIAN_POINT('Ctrl Pts',(-9.85692793745532,1.7408939537672,-8.60247731152257));
#6838=CARTESIAN_POINT('Ctrl Pts',(-9.77133803228051,2.16990305716179,-8.30002077297609));
#6839=CARTESIAN_POINT('Ctrl Pts',(-9.65925826289068,2.58819045102525,-8.));
#6840=CARTESIAN_POINT('',(-9.65925826289068,2.58819045102525,8.));
#6841=CARTESIAN_POINT('',(-9.65925826289068,2.58819045102525,30.));
#6842=CARTESIAN_POINT('',(-10.0001237867953,1.97103495948311E-9,9.76179717313037));
#6843=CARTESIAN_POINT('Ctrl Pts',(-9.65925826289068,2.58819045102525,8.));
#6844=CARTESIAN_POINT('Ctrl Pts',(-9.77163928663693,2.16877876059763,8.30082718581888));
#6845=CARTESIAN_POINT('Ctrl Pts',(-9.85693279744154,1.74086457562841,8.60249771169349));
#6846=CARTESIAN_POINT('Ctrl Pts',(-9.97097123275185,0.877192293395072,9.1931881535409));
#6847=CARTESIAN_POINT('Ctrl Pts',(-10.,0.441537174494764,9.48227427600301));
#6848=CARTESIAN_POINT('Ctrl Pts',(-10.,3.58012987980397E-8,9.76179723440599));
#6849=CARTESIAN_POINT('Ctrl Pts',(-10.0001819091909,-1.39135025250588E-8,
9.76179714435925));
#6850=CARTESIAN_POINT('Ctrl Pts',(-10.0002422168267,-0.190993084247708,
9.88270644163236));
#6851=CARTESIAN_POINT('Ctrl Pts',(-9.99480220281986,-0.383077493992189,
10.00183306457));
#6852=CARTESIAN_POINT('Ctrl Pts',(-9.98359703547028,-0.576510028433417,
10.118774303758));
#6853=CARTESIAN_POINT('Ctrl Pts',(-9.97256127034954,-0.767018206509035,
10.2339475991086));
#6854=CARTESIAN_POINT('Ctrl Pts',(-9.95593360360136,-0.95883449076797,10.3470012231726));
#6855=CARTESIAN_POINT('Ctrl Pts',(-9.93344119546686,-1.15222238942891,10.4575076433073));
#6856=CARTESIAN_POINT('Ctrl Pts',(-9.9262367904895,-1.21416527839578,10.4929032754017));
#6857=CARTESIAN_POINT('Ctrl Pts',(-9.91843052664459,-1.27626951880198,10.5280372367801));
#6858=CARTESIAN_POINT('Ctrl Pts',(-9.91001294263524,-1.33854404163207,10.562894487102));
#6859=CARTESIAN_POINT('Ctrl Pts',(-9.90749042320113,-1.35720601089949,10.5733402505489));
#6860=CARTESIAN_POINT('Ctrl Pts',(-9.90491108546458,-1.37589744516174,10.5837694597516));
#6861=CARTESIAN_POINT('Ctrl Pts',(-9.90227459651842,-1.39461744436323,10.5941810273423));
#6862=CARTESIAN_POINT('Ctrl Pts',(-9.8852516513421,-1.51548634486515,10.6614051075165));
#6863=CARTESIAN_POINT('Ctrl Pts',(-9.86586922292159,-1.63704928825616,10.7275744442729));
#6864=CARTESIAN_POINT('Ctrl Pts',(-9.84409332992305,-1.75891940227426,10.7922898679902));
#6865=CARTESIAN_POINT('Ctrl Pts',(-9.82820853223256,-1.84781964190271,10.8394976409744));
#6866=CARTESIAN_POINT('Ctrl Pts',(-9.81105101031158,-1.93688317128088,10.8859320635458));
#6867=CARTESIAN_POINT('Ctrl Pts',(-9.79262273697897,-2.02595889184268,10.9314471311979));
#6868=CARTESIAN_POINT('Ctrl Pts',(-9.76488031347849,-2.16005590238909,10.9999667510052));
#6869=CARTESIAN_POINT('Ctrl Pts',(-9.73425070221459,-2.29422898087712,11.0664231571024));
#6870=CARTESIAN_POINT('Ctrl Pts',(-9.70066935863215,-2.42837682308185,11.1305171637201));
#6871=CARTESIAN_POINT('Ctrl Pts',(-9.67662805956223,-2.52441492191826,11.1764028555152));
#6872=CARTESIAN_POINT('Ctrl Pts',(-9.65106802401281,-2.62050374832403,11.2211217985967));
#6873=CARTESIAN_POINT('Ctrl Pts',(-9.62392825897893,-2.71666946271822,11.2645470181033));
#6874=CARTESIAN_POINT('Ctrl Pts',(-9.58471316352384,-2.85562231160131,11.3272934761505));
#6875=CARTESIAN_POINT('Ctrl Pts',(-9.5422477893575,-2.9945749698244,11.387297557256));
#6876=CARTESIAN_POINT('Ctrl Pts',(-9.49630917584708,-3.13375936775937,11.4442500498319));
#6877=CARTESIAN_POINT('Ctrl Pts',(-9.46066803283884,-3.24174458220626,11.488436231727));
#6878=CARTESIAN_POINT('Ctrl Pts',(-9.42293563050879,-3.34986928377481,11.5307850355101));
#6879=CARTESIAN_POINT('Ctrl Pts',(-9.3829931498531,-3.45824226410632,11.5711359915397));
#6880=CARTESIAN_POINT('Ctrl Pts',(-9.33776999970747,-3.58094289463323,11.6168216203012));
#6881=CARTESIAN_POINT('Ctrl Pts',(-9.28952854437317,-3.70428222851569,11.6600098053998));
#6882=CARTESIAN_POINT('Ctrl Pts',(-9.23831661995914,-3.82783387752058,11.7001335892842));
#6883=CARTESIAN_POINT('Ctrl Pts',(-9.19964613725768,-3.92112859276999,11.7304313394346));
#6884=CARTESIAN_POINT('Ctrl Pts',(-9.15928155479108,-4.01454418176179,11.7589811573433));
#6885=CARTESIAN_POINT('Ctrl Pts',(-9.11723772204827,-4.10788860814096,11.7855218310166));
#6886=CARTESIAN_POINT('Ctrl Pts',(-9.06035407011132,-4.23417994539576,11.8214303185383));
#6887=CARTESIAN_POINT('Ctrl Pts',(-9.00060480640979,-4.35987805857573,11.8535369691633));
#6888=CARTESIAN_POINT('Ctrl Pts',(-8.93810575967581,-4.4844470594322,11.8812385781177));
#6889=CARTESIAN_POINT('Ctrl Pts',(-8.8655173877299,-4.62912544157758,11.9134121039451));
#6890=CARTESIAN_POINT('Ctrl Pts',(-8.78916153683245,-4.7726019250157,11.9398813478119));
#6891=CARTESIAN_POINT('Ctrl Pts',(-8.70881072233522,-4.91498224698192,11.9596101136812));
#6892=CARTESIAN_POINT('Ctrl Pts',(-8.63305448011727,-5.04922106242435,11.9782107610451));
#6893=CARTESIAN_POINT('Ctrl Pts',(-8.55374701687845,-5.1824854269134,11.9908200299044));
#6894=CARTESIAN_POINT('Ctrl Pts',(-8.4706795483874,-5.31485894338431,11.9965268972474));
#6895=CARTESIAN_POINT('Ctrl Pts',(-8.4372756670212,-5.36809024223746,11.9988217970819));
#6896=CARTESIAN_POINT('Ctrl Pts',(-8.40326355436336,-5.42117742990113,11.9999999989612));
#6897=CARTESIAN_POINT('Ctrl Pts',(-8.36862877099654,-5.47412572866653,12.));
#6898=CARTESIAN_POINT('',(10.,-1.22464679914735E-15,15.));
#6899=CARTESIAN_POINT('',(10.,-1.22464679914735E-15,30.));
#6900=CARTESIAN_POINT('Origin',(0.,0.,15.));
#6901=CARTESIAN_POINT('',(0.,10.,8.));
#6902=CARTESIAN_POINT('Ctrl Pts',(7.4535599249993,6.66666666666667,12.));
#6903=CARTESIAN_POINT('Ctrl Pts',(7.32443309352201,6.81103485311786,11.99999999682));
#6904=CARTESIAN_POINT('Ctrl Pts',(7.19246919567612,6.9501822010365,11.9889588601183));
#6905=CARTESIAN_POINT('Ctrl Pts',(7.0576993924076,7.08444300037639,11.9685994397917));
#6906=CARTESIAN_POINT('Ctrl Pts',(6.92292958913909,7.21870379971628,11.9482400194651));
#6907=CARTESIAN_POINT('Ctrl Pts',(6.78535384384508,7.34807802019908,11.9185618083842));
#6908=CARTESIAN_POINT('Ctrl Pts',(6.64499605849823,7.47288614812075,11.8812318773614));
#6909=CARTESIAN_POINT('Ctrl Pts',(6.63654366979561,7.48040213170394,11.8789838575137));
#6910=CARTESIAN_POINT('Ctrl Pts',(6.62807974800606,7.48790223671562,11.8767069196995));
#6911=CARTESIAN_POINT('Ctrl Pts',(6.61960457791775,7.49538631823325,11.8744014042209));
#6912=CARTESIAN_POINT('Ctrl Pts',(6.48185055268487,7.61703135231309,11.8369279335891));
#6913=CARTESIAN_POINT('Ctrl Pts',(6.34120540493964,7.73437093825154,11.791921326457));
#6914=CARTESIAN_POINT('Ctrl Pts',(6.19898657325189,7.84672900130041,11.7408838129976));
#6915=CARTESIAN_POINT('Ctrl Pts',(6.05676774156413,7.95908706434928,11.6898462995382));
#6916=CARTESIAN_POINT('Ctrl Pts',(5.9129759592346,8.06646321098892,11.6327787221492));
#6917=CARTESIAN_POINT('Ctrl Pts',(5.76889672089669,8.16822077470328,11.571161743219));
#6918=CARTESIAN_POINT('Ctrl Pts',(5.75379442418606,8.1788869396379,11.5647030895716));
#6919=CARTESIAN_POINT('Ctrl Pts',(5.73868373288969,8.18949663728534,11.5581931861037));
#6920=CARTESIAN_POINT('Ctrl Pts',(5.72356470502882,8.2000502330104,11.5516328635545));
#6921=CARTESIAN_POINT('Ctrl Pts',(5.54237464595592,8.32652705747638,11.4730123833783));
#6922=CARTESIAN_POINT('Ctrl Pts',(5.35972864022817,8.44512957455917,11.3870622034709));
#6923=CARTESIAN_POINT('Ctrl Pts',(5.17553266659185,8.55653116699126,11.2950285747769));
#6924=CARTESIAN_POINT('Ctrl Pts',(5.06965587040675,8.6205653772065,11.2421271700663));
#6925=CARTESIAN_POINT('Ctrl Pts',(4.96326699017399,8.68221979432739,11.18721494629));
#6926=CARTESIAN_POINT('Ctrl Pts',(4.85634813127281,8.7416178610103,11.1305223120243));
#6927=CARTESIAN_POINT('Ctrl Pts',(4.83760485921073,8.75203056214872,11.1205838832113));
#6928=CARTESIAN_POINT('Ctrl Pts',(4.81884248159145,8.76237495465752,11.1105886554459));
#6929=CARTESIAN_POINT('Ctrl Pts',(4.80006143083322,8.77265117277875,11.1005377116491));
#6930=CARTESIAN_POINT('Ctrl Pts',(4.67853878586853,8.83914336335964,11.035503156858));
#6931=CARTESIAN_POINT('Ctrl Pts',(4.55611379988328,8.9028432066626,10.9680753730249));
#6932=CARTESIAN_POINT('Ctrl Pts',(4.43314656586013,8.96365874967832,10.8986785149911));
#6933=CARTESIAN_POINT('Ctrl Pts',(4.30539927968577,9.02683834901789,10.8265840228829));
#6934=CARTESIAN_POINT('Ctrl Pts',(4.17706707175951,9.08690480285482,10.7523650450191));
#6935=CARTESIAN_POINT('Ctrl Pts',(4.04856409267038,9.14380227472548,10.6765257027452));
#6936=CARTESIAN_POINT('Ctrl Pts',(4.0023909454348,9.16424643379976,10.6492754308691));
#6937=CARTESIAN_POINT('Ctrl Pts',(3.95619582194605,9.1842818998028,10.6218161673034));
#6938=CARTESIAN_POINT('Ctrl Pts',(3.90999812363261,9.2039075764655,10.5941718862756));
#6939=CARTESIAN_POINT('Ctrl Pts',(3.8904775206927,9.21220030652664,10.5824909356394));
#6940=CARTESIAN_POINT('Ctrl Pts',(3.87097075026249,9.22041521797258,10.5707865416166));
#6941=CARTESIAN_POINT('Ctrl Pts',(3.85147861510306,9.22855261214377,10.559059913264));
#6942=CARTESIAN_POINT('Ctrl Pts',(3.60036010696405,9.33338721685456,10.4079849595288));
#6943=CARTESIAN_POINT('Ctrl Pts',(3.34928636559173,9.42635559679678,10.2518372325069));
#6944=CARTESIAN_POINT('Ctrl Pts',(3.09786269543073,9.50831050937557,10.0916156638059));
#6945=CARTESIAN_POINT('Ctrl Pts',(2.83364682712233,9.59443521026502,9.92324217347811));
#6946=CARTESIAN_POINT('Ctrl Pts',(2.56904501266554,9.66839715764356,9.75036930809004));
#6947=CARTESIAN_POINT('Ctrl Pts',(2.30359960581663,9.73113308394545,9.57413333089425));
#6948=CARTESIAN_POINT('Ctrl Pts',(2.19421189175197,9.75698600658351,9.50150803701462));
#6949=CARTESIAN_POINT('Ctrl Pts',(2.08468088072785,9.7809319426623,9.42831140146962));
#6950=CARTESIAN_POINT('Ctrl Pts',(1.974974279851,9.80303405043287,9.35462218793377));
#6951=CARTESIAN_POINT('Ctrl Pts',(1.9634639600312,9.80535298408953,9.34689078063204));
#6952=CARTESIAN_POINT('Ctrl Pts',(1.9519511325459,9.80765144332111,9.33915328863826));
#6953=CARTESIAN_POINT('Ctrl Pts',(1.94043581192868,9.80992942994645,9.33140979991383));
#6954=CARTESIAN_POINT('Ctrl Pts',(1.76247768584885,9.84513350671991,9.21174168223595));
#6955=CARTESIAN_POINT('Ctrl Pts',(1.58405644832137,9.87542603772905,9.09072486559958));
#6956=CARTESIAN_POINT('Ctrl Pts',(1.40504595874219,9.90084697353231,8.96857634820572));
#6957=CARTESIAN_POINT('Ctrl Pts',(1.26163873401112,9.92121195807696,8.87072185975843));
#6958=CARTESIAN_POINT('Ctrl Pts',(1.11785322956714,9.93844951919808,8.77214041219644));
#6959=CARTESIAN_POINT('Ctrl Pts',(0.973624298149134,9.95255818426511,8.67293388154916));
#6960=CARTESIAN_POINT('Ctrl Pts',(0.82272776139333,9.96731908331589,8.56914110050965));
#6961=CARTESIAN_POINT('Ctrl Pts',(0.671530069329876,9.97863100442017,8.46479064327355));
#6962=CARTESIAN_POINT('Ctrl Pts',(0.520367904445434,9.98649236040718,8.36027671301796));
#6963=CARTESIAN_POINT('Ctrl Pts',(0.368186462519023,9.99440672502689,8.25505805185462));
#6964=CARTESIAN_POINT('Ctrl Pts',(0.216041172145373,9.99882382364899,8.14967421046749));
#6965=CARTESIAN_POINT('Ctrl Pts',(0.0642766288123017,9.99979448577473,8.04453172419152));
#6966=CARTESIAN_POINT('Ctrl Pts',(0.0428431687350635,9.99993157081095,8.02968262154525));
#6967=CARTESIAN_POINT('Ctrl Pts',(0.0214173025071013,10.,8.01483833249367));
#6968=CARTESIAN_POINT('Ctrl Pts',(1.33226762955019E-15,10.,8.));
#6969=CARTESIAN_POINT('',(0.,10.,-8.));
#6970=CARTESIAN_POINT('',(0.,10.,30.));
#6971=CARTESIAN_POINT('',(7.4535599249993,6.66666666666667,-12.));
#6972=CARTESIAN_POINT('Ctrl Pts',(0.,10.,-8.));
#6973=CARTESIAN_POINT('Ctrl Pts',(0.209085099686919,10.,-8.14485830919264));
#6974=CARTESIAN_POINT('Ctrl Pts',(0.418288781390105,9.99347420733504,-8.28980641296881));
#6975=CARTESIAN_POINT('Ctrl Pts',(0.627262534901026,9.98035857777825,-8.43416422574658));
#6976=CARTESIAN_POINT('Ctrl Pts',(0.847178419334319,9.96655619721408,-8.58608079679203));
#6977=CARTESIAN_POINT('Ctrl Pts',(1.06683943516283,9.94545528423446,-8.73734285597004));
#6978=CARTESIAN_POINT('Ctrl Pts',(1.28584122492737,9.91704302479201,-8.88715246988158));
#6979=CARTESIAN_POINT('Ctrl Pts',(1.49281407510468,9.89019134324591,-9.02873360859543));
#6980=CARTESIAN_POINT('Ctrl Pts',(1.69919797291203,9.85680994096409,-9.16901679075694));
#6981=CARTESIAN_POINT('Ctrl Pts',(1.90465594999555,9.81694004719906,-9.30733474421298));
#6982=CARTESIAN_POINT('Ctrl Pts',(1.91659684751875,9.814622871091,-9.31537356816755));
#6983=CARTESIAN_POINT('Ctrl Pts',(1.9285346191681,9.81228379261445,-9.32340575754666));
#6984=CARTESIAN_POINT('Ctrl Pts',(1.94046919944125,9.80992282509999,-9.33143118277434));
#6985=CARTESIAN_POINT('Ctrl Pts',(1.95197352173875,9.80764697370023,-9.33916728042341));
#6986=CARTESIAN_POINT('Ctrl Pts',(1.96347535561302,9.80535068876919,-9.34689739267515));
#6987=CARTESIAN_POINT('Ctrl Pts',(1.97497468657832,9.80303396849238,-9.35462143181174));
#6988=CARTESIAN_POINT('Ctrl Pts',(2.24251254824573,9.74913427721365,-9.53432518329739));
#6989=CARTESIAN_POINT('Ctrl Pts',(2.5090065924052,9.68427253191354,-9.71110047463118));
#6990=CARTESIAN_POINT('Ctrl Pts',(2.7749232834884,9.60751844470339,-9.88380087138435));
#6991=CARTESIAN_POINT('Ctrl Pts',(3.02784790867845,9.5345143821891,-10.0480635317726));
#6992=CARTESIAN_POINT('Ctrl Pts',(3.28024979088569,9.45075168409379,-10.2086402039897));
#6993=CARTESIAN_POINT('Ctrl Pts',(3.53252798197937,9.35538605373282,-10.3645278522479));
#6994=CARTESIAN_POINT('Ctrl Pts',(3.6388640692924,9.31518912686901,-10.4302350087181));
#6995=CARTESIAN_POINT('Ctrl Pts',(3.74517818821727,9.2729302095569,-10.4951088432616));
#6996=CARTESIAN_POINT('Ctrl Pts',(3.85150038699593,9.22854352298752,-10.5590730208312));
#6997=CARTESIAN_POINT('Ctrl Pts',(3.87098527378687,9.22040910164594,-10.5707952648493));
#6998=CARTESIAN_POINT('Ctrl Pts',(3.89048478576427,9.21219722017683,-10.5824952913507));
#6999=CARTESIAN_POINT('Ctrl Pts',(3.9099981209759,9.20390757759402,-10.5941718925655));
#7000=CARTESIAN_POINT('Ctrl Pts',(4.03898075658645,9.14911325683834,-10.6713539213333));
#7001=CARTESIAN_POINT('Ctrl Pts',(4.16794297285713,9.09112109034215,-10.7470924847379));
#7002=CARTESIAN_POINT('Ctrl Pts',(4.29646417587719,9.02997028952467,-10.8208712485592));
#7003=CARTESIAN_POINT('Ctrl Pts',(4.42014485896863,8.97112262362231,-10.8918712679539));
#7004=CARTESIAN_POINT('Ctrl Pts',(4.54341682842248,8.90934998996412,-10.9610556950588));
#7005=CARTESIAN_POINT('Ctrl Pts',(4.66591280664953,8.84472972017589,-11.0279859964137));
#7006=CARTESIAN_POINT('Ctrl Pts',(4.71074408320321,8.82107988915467,-11.0524812565299));
#7007=CARTESIAN_POINT('Ctrl Pts',(4.75547151809011,8.79704904424051,-11.0766748545963));
#7008=CARTESIAN_POINT('Ctrl Pts',(4.80007749004456,8.77264238582005,-11.1005463067514));
#7009=CARTESIAN_POINT('Ctrl Pts',(4.81885317713414,8.76236905780305,-11.1105943540508));
#7010=CARTESIAN_POINT('Ctrl Pts',(4.8376102014733,8.7520275942893,-11.1205867167142));
#7011=CARTESIAN_POINT('Ctrl Pts',(4.85634813102705,8.74161786114682,-11.1305223127522));
#7012=CARTESIAN_POINT('Ctrl Pts',(5.04235190637572,8.63828469088813,-11.229148917581));
#7013=CARTESIAN_POINT('Ctrl Pts',(5.22675176126298,8.5281243719752,-11.32238944137));
#7014=CARTESIAN_POINT('Ctrl Pts',(5.40964172666946,8.41048088884993,-11.40902216654));
#7015=CARTESIAN_POINT('Ctrl Pts',(5.51477922677033,8.34285147194091,-11.4588245060564));
#7016=CARTESIAN_POINT('Ctrl Pts',(5.61941772167317,8.27274856573666,-11.5064424239632));
#7017=CARTESIAN_POINT('Ctrl Pts',(5.72357511243166,8.20004296827939,-11.5516373819622));
#7018=CARTESIAN_POINT('Ctrl Pts',(5.73869066712922,8.18949176853081,-11.5581961758674));
#7019=CARTESIAN_POINT('Ctrl Pts',(5.75379788912304,8.17888449248633,-11.5647045736646));
#7020=CARTESIAN_POINT('Ctrl Pts',(5.76889672042948,8.16822077503325,-11.5711617451841));
#7021=CARTESIAN_POINT('Ctrl Pts',(5.91297681932932,8.06646260354981,-11.6327790910746));
#7022=CARTESIAN_POINT('Ctrl Pts',(6.05676946305485,7.95908577894731,-11.6898469834438));
#7023=CARTESIAN_POINT('Ctrl Pts',(6.19898913169897,7.84672698003327,-11.740884731588));
#7024=CARTESIAN_POINT('Ctrl Pts',(6.34120880034308,7.73436818111923,-11.7919224797322));
#7025=CARTESIAN_POINT('Ctrl Pts',(6.48185476056317,7.61702780143568,-11.8369292412042));
#7026=CARTESIAN_POINT('Ctrl Pts',(6.61960954778086,7.49538192954424,-11.874402757394));
#7027=CARTESIAN_POINT('Ctrl Pts',(6.62808305681875,7.48789930468805,-11.8767078110661));
#7028=CARTESIAN_POINT('Ctrl Pts',(6.63654532187993,7.48040066264689,-11.8789842981708));
#7029=CARTESIAN_POINT('Ctrl Pts',(6.64499605834415,7.47288614825776,-11.8812318786062));
#7030=CARTESIAN_POINT('Ctrl Pts',(6.78535384876212,7.34807801583195,-11.9185618113333));
#7031=CARTESIAN_POINT('Ctrl Pts',(6.92292959388377,7.21870379512185,-11.9482400216728));
#7032=CARTESIAN_POINT('Ctrl Pts',(7.05769939588734,7.08444299690985,-11.9685994412462));
#7033=CARTESIAN_POINT('Ctrl Pts',(7.1924691978909,6.95018219869785,-11.9889588608196));
#7034=CARTESIAN_POINT('Ctrl Pts',(7.32443309337662,6.8110348532804,-11.99999999682));
#7035=CARTESIAN_POINT('Ctrl Pts',(7.4535599249993,6.66666666666667,-12.));
#7036=CARTESIAN_POINT('Origin',(0.,0.,-12.));
#7037=CARTESIAN_POINT('Origin',(0.,0.,10.));
#7038=CARTESIAN_POINT('',(-18.0801684144135,-36.5664806907425,10.));
#7039=CARTESIAN_POINT('',(-18.0801684144135,-36.5664806907425,10.));
#7040=CARTESIAN_POINT('',(-2.62535519378845,-40.7075854123829,10.));
#7041=CARTESIAN_POINT('Origin',(-10.352761804101,-38.6370330515627,10.));
#7042=CARTESIAN_POINT('',(1.76944146100923,-24.3059810077445,10.));
#7043=CARTESIAN_POINT('',(1.76944146100923,-24.3059810077445,10.));
#7044=CARTESIAN_POINT('',(23.0198096393687,-8.,10.));
#7045=CARTESIAN_POINT('Origin',(23.0198096393687,-30.,10.));
#7046=CARTESIAN_POINT('',(45.,-8.,10.));
#7047=CARTESIAN_POINT('',(47.,-8.,10.));
#7048=CARTESIAN_POINT('',(45.,8.,10.));
#7049=CARTESIAN_POINT('',(45.,1.56125112837913E-14,10.));
#7050=CARTESIAN_POINT('',(3.69090101271661E-16,8.,10.));
#7051=CARTESIAN_POINT('Origin',(-9.65925826289068,2.58819045102525,30.));
#7052=CARTESIAN_POINT('',(-9.65925826289068,2.58819045102525,8.));
#7053=CARTESIAN_POINT('',(-20.0120200669917,-36.0488426005374,-8.));
#7054=CARTESIAN_POINT('',(-15.8709153453513,-20.5940293799124,-5.));
#7055=CARTESIAN_POINT('',(-15.8709153453513,-20.5940293799124,-5.));
#7056=CARTESIAN_POINT('',(-15.8709153453513,-20.5940293799124,5.));
#7057=CARTESIAN_POINT('',(-15.8709153453513,-20.5940293799124,5.));
#7058=CARTESIAN_POINT('',(-15.8709153453513,-20.5940293799124,5.));
#7059=CARTESIAN_POINT('Origin',(-0.693503541210314,-41.2252235025879,30.));
#7060=CARTESIAN_POINT('',(3.70129311358736,-24.8236190979495,8.));
#7061=CARTESIAN_POINT('',(3.70129311358736,-24.8236190979495,-8.));
#7062=CARTESIAN_POINT('',(3.70129311358736,-24.8236190979495,30.));
#7063=CARTESIAN_POINT('',(-0.693503541210312,-41.2252235025879,8.));
#7064=CARTESIAN_POINT('',(3.44760118043008,-25.7704102819629,5.));
#7065=CARTESIAN_POINT('',(-0.693503541210314,-41.2252235025879,5.));
#7066=CARTESIAN_POINT('',(3.44760118043008,-25.7704102819629,-5.));
#7067=CARTESIAN_POINT('',(3.44760118043008,-25.7704102819629,5.));
#7068=CARTESIAN_POINT('',(-0.693503541210314,-41.2252235025879,-5.));
#7069=CARTESIAN_POINT('',(3.70129311358736,-24.8236190979495,-8.));
#7070=CARTESIAN_POINT('Origin',(23.0198096393687,-30.,30.));
#7071=CARTESIAN_POINT('',(23.0198096393687,-10.,8.));
#7072=CARTESIAN_POINT('',(23.0198096393687,-10.,-8.));
#7073=CARTESIAN_POINT('',(23.0198096393687,-10.,30.));
#7074=CARTESIAN_POINT('Origin',(23.0198096393687,-30.,8.));
#7075=CARTESIAN_POINT('Origin',(23.0198096393687,-30.,-8.));
#7076=CARTESIAN_POINT('Origin',(23.0198096393687,-10.,30.));
#7077=CARTESIAN_POINT('',(80.,-10.,22.));
#7078=CARTESIAN_POINT('',(80.,-10.,30.));
#7079=CARTESIAN_POINT('',(54.,-10.,28.));
#7080=CARTESIAN_POINT('',(54.,-10.,28.));
#7081=CARTESIAN_POINT('',(49.,-10.,23.));
#7082=CARTESIAN_POINT('Origin',(54.,-10.,23.));
#7083=CARTESIAN_POINT('',(49.,-10.,12.));
#7084=CARTESIAN_POINT('',(49.,-10.,30.));
#7085=CARTESIAN_POINT('',(45.,-10.,8.));
#7086=CARTESIAN_POINT('Origin',(45.,-10.,12.));
#7087=CARTESIAN_POINT('',(23.0198096393687,-10.,8.));
#7088=CARTESIAN_POINT('',(45.,-10.,-8.));
#7089=CARTESIAN_POINT('',(47.,-10.,-8.));
#7090=CARTESIAN_POINT('',(49.,-10.,-12.));
#7091=CARTESIAN_POINT('Origin',(45.,-10.,-12.));
#7092=CARTESIAN_POINT('',(49.,-10.,-23.));
#7093=CARTESIAN_POINT('',(49.,-10.,30.));
#7094=CARTESIAN_POINT('',(54.,-10.,-28.));
#7095=CARTESIAN_POINT('Origin',(54.,-10.,-23.));
#7096=CARTESIAN_POINT('',(80.,-10.,-28.));
#7097=CARTESIAN_POINT('',(80.,-10.,-28.));
#7098=CARTESIAN_POINT('',(80.,-10.,-22.));
#7099=CARTESIAN_POINT('',(80.,-10.,-30.));
#7100=CARTESIAN_POINT('',(54.,-10.,-22.));
#7101=CARTESIAN_POINT('',(54.,-10.,-22.));
#7102=CARTESIAN_POINT('',(54.,-10.,22.));
#7103=CARTESIAN_POINT('',(54.,-10.,22.));
#7104=CARTESIAN_POINT('',(54.,-10.,22.));
#7105=CARTESIAN_POINT('Origin',(0.,10.,30.));
#7106=CARTESIAN_POINT('',(49.,10.,23.));
#7107=CARTESIAN_POINT('',(54.,10.,28.));
#7108=CARTESIAN_POINT('Origin',(54.,10.,23.));
#7109=CARTESIAN_POINT('',(80.,10.,28.));
#7110=CARTESIAN_POINT('',(80.,10.,22.));
#7111=CARTESIAN_POINT('',(80.,10.,30.));
#7112=CARTESIAN_POINT('',(54.,10.,22.));
#7113=CARTESIAN_POINT('',(80.,10.,22.));
#7114=CARTESIAN_POINT('',(54.,10.,-22.));
#7115=CARTESIAN_POINT('',(54.,10.,22.));
#7116=CARTESIAN_POINT('',(80.,10.,-22.));
#7117=CARTESIAN_POINT('',(80.,10.,-22.));
#7118=CARTESIAN_POINT('',(80.,10.,-28.));
#7119=CARTESIAN_POINT('',(80.,10.,-30.));
#7120=CARTESIAN_POINT('',(54.,10.,-28.));
#7121=CARTESIAN_POINT('',(54.,10.,-28.));
#7122=CARTESIAN_POINT('',(49.,10.,-23.));
#7123=CARTESIAN_POINT('Origin',(54.,10.,-23.));
#7124=CARTESIAN_POINT('',(49.,10.,-12.));
#7125=CARTESIAN_POINT('',(49.,10.,30.));
#7126=CARTESIAN_POINT('',(45.,10.,-8.));
#7127=CARTESIAN_POINT('Origin',(45.,10.,-12.));
#7128=CARTESIAN_POINT('',(3.69090101271661E-16,10.,-8.));
#7129=CARTESIAN_POINT('',(45.,10.,8.));
#7130=CARTESIAN_POINT('',(47.,10.,8.));
#7131=CARTESIAN_POINT('',(49.,10.,12.));
#7132=CARTESIAN_POINT('Origin',(45.,10.,12.));
#7133=CARTESIAN_POINT('',(49.,10.,30.));
#7134=CARTESIAN_POINT('Origin',(0.,0.,30.));
#7135=CARTESIAN_POINT('',(54.,8.,30.));
#7136=CARTESIAN_POINT('',(54.,-8.,30.));
#7137=CARTESIAN_POINT('',(54.,-10.,30.));
#7138=CARTESIAN_POINT('',(80.,-8.,30.));
#7139=CARTESIAN_POINT('',(54.,8.,30.));
#7140=CARTESIAN_POINT('Origin',(80.,0.,30.));
#7141=CARTESIAN_POINT('Origin',(80.,0.,22.));
#7142=CARTESIAN_POINT('Origin',(54.,10.,22.));
#7143=CARTESIAN_POINT('',(54.,10.,-22.));
#7144=CARTESIAN_POINT('',(54.,10.,22.));
#7145=CARTESIAN_POINT('Origin',(80.,0.,22.));
#7146=CARTESIAN_POINT('Origin',(-15.8709153453513,-20.5940293799124,5.));
#7147=CARTESIAN_POINT('',(-15.8709153453513,-20.5940293799124,-5.));
#7148=CARTESIAN_POINT('',(-15.8709153453513,-20.5940293799124,5.));
#7149=CARTESIAN_POINT('Origin',(-10.352761804101,-38.6370330515627,5.));
#7150=CARTESIAN_POINT('Origin',(47.,10.,10.));
#7151=CARTESIAN_POINT('',(47.,-8.,23.));
#7152=CARTESIAN_POINT('',(47.,8.,23.));
#7153=CARTESIAN_POINT('',(47.,10.,23.));
#7154=CARTESIAN_POINT('',(47.,8.,12.));
#7155=CARTESIAN_POINT('',(47.,8.,10.));
#7156=CARTESIAN_POINT('',(47.,-8.,12.));
#7157=CARTESIAN_POINT('',(47.,10.,12.));
#7158=CARTESIAN_POINT('',(47.,-8.,10.));
#7159=CARTESIAN_POINT('Origin',(0.,0.,15.));
#7160=CARTESIAN_POINT('Origin',(0.,0.,-10.));
#7161=CARTESIAN_POINT('',(1.76944146100923,-24.3059810077445,-10.));
#7162=CARTESIAN_POINT('',(-2.62535519378845,-40.7075854123829,-10.));
#7163=CARTESIAN_POINT('',(-10.0423545251959,-6.56895087439983,-10.));
#7164=CARTESIAN_POINT('',(-7.72740661031254,2.0705523608202,-10.));
#7165=CARTESIAN_POINT('',(8.94427190999916,8.,-10.));
#7166=CARTESIAN_POINT('Origin',(0.,0.,-10.));
#7167=CARTESIAN_POINT('',(45.,8.,-10.));
#7168=CARTESIAN_POINT('',(47.,8.,-10.));
#7169=CARTESIAN_POINT('',(45.,-8.,-10.));
#7170=CARTESIAN_POINT('',(45.,1.56125112837913E-14,-10.));
#7171=CARTESIAN_POINT('',(23.0198096393687,-8.,-10.));
#7172=CARTESIAN_POINT('',(23.0198096393687,-8.,-10.));
#7173=CARTESIAN_POINT('Origin',(23.0198096393687,-30.,-10.));
#7174=CARTESIAN_POINT('Origin',(0.,0.,-30.));
#7175=CARTESIAN_POINT('',(80.,8.,-30.));
#7176=CARTESIAN_POINT('',(80.,-8.,-30.));
#7177=CARTESIAN_POINT('Origin',(80.,0.,-30.));
#7178=CARTESIAN_POINT('',(54.,-8.,-30.));
#7179=CARTESIAN_POINT('',(54.,-8.,-30.));
#7180=CARTESIAN_POINT('',(54.,8.,-30.));
#7181=CARTESIAN_POINT('',(54.,10.,-30.));
#7182=CARTESIAN_POINT('',(80.,8.,-30.));
#7183=CARTESIAN_POINT('Origin',(80.,0.,-30.));
#7184=CARTESIAN_POINT('Origin',(80.,0.,-28.));
#7185=CARTESIAN_POINT('Origin',(80.,0.,-22.));
#7186=CARTESIAN_POINT('Origin',(80.,0.,-22.));
#7187=CARTESIAN_POINT('Origin',(-10.352761804101,-38.6370330515627,-5.));
#7188=CARTESIAN_POINT('Origin',(47.,10.,-10.));
#7189=CARTESIAN_POINT('',(47.,8.,-23.));
#7190=CARTESIAN_POINT('',(47.,-8.,-23.));
#7191=CARTESIAN_POINT('',(47.,-10.,-23.));
#7192=CARTESIAN_POINT('',(47.,-8.,-12.));
#7193=CARTESIAN_POINT('',(47.,-8.,-10.));
#7194=CARTESIAN_POINT('',(47.,8.,-12.));
#7195=CARTESIAN_POINT('',(47.,10.,-12.));
#7196=CARTESIAN_POINT('',(47.,8.,-10.));
#7197=CARTESIAN_POINT('Origin',(0.,0.,-15.));
#7198=CARTESIAN_POINT('Origin',(54.,1.87350135405495E-14,-23.));
#7199=CARTESIAN_POINT('Origin',(54.,-8.,-23.));
#7200=CARTESIAN_POINT('Origin',(54.,8.,-23.));
#7201=CARTESIAN_POINT('Origin',(54.,10.,23.));
#7202=CARTESIAN_POINT('Origin',(54.,8.,23.));
#7203=CARTESIAN_POINT('Origin',(54.,-8.,23.));
#7204=CARTESIAN_POINT('Origin',(0.,8.,28.));
#7205=CARTESIAN_POINT('Origin',(54.,8.,28.));
#7206=CARTESIAN_POINT('Origin',(-4.8710921181488E-16,-8.,28.));
#7207=CARTESIAN_POINT('Origin',(54.,-8.,28.));
#7208=CARTESIAN_POINT('Origin',(54.,8.,23.));
#7209=CARTESIAN_POINT('Origin',(49.,8.,23.));
#7210=CARTESIAN_POINT('Origin',(54.,-8.,23.));
#7211=CARTESIAN_POINT('Origin',(49.,-8.,23.));
#7212=CARTESIAN_POINT('Origin',(49.,8.,30.));
#7213=CARTESIAN_POINT('Origin',(49.,8.,12.));
#7214=CARTESIAN_POINT('Origin',(45.,1.56125112837913E-14,12.));
#7215=CARTESIAN_POINT('Origin',(45.,-8.,12.));
#7216=CARTESIAN_POINT('Origin',(45.,8.,12.));
#7217=CARTESIAN_POINT('Origin',(49.,-8.,10.));
#7218=CARTESIAN_POINT('Origin',(49.,-8.,12.));
#7219=CARTESIAN_POINT('Origin',(45.,8.,12.));
#7220=CARTESIAN_POINT('Origin',(45.,8.,8.));
#7221=CARTESIAN_POINT('Origin',(45.,-8.,12.));
#7222=CARTESIAN_POINT('Origin',(45.,-8.,8.));
#7223=CARTESIAN_POINT('Origin',(0.,8.,8.));
#7224=CARTESIAN_POINT('Ctrl Pts',(8.94427190999916,8.,10.));
#7225=CARTESIAN_POINT('Ctrl Pts',(8.59397428869209,8.19582232339978,10.));
#7226=CARTESIAN_POINT('Ctrl Pts',(8.23809574830832,8.36927906280638,9.97233221567645));
#7227=CARTESIAN_POINT('Ctrl Pts',(7.51670439182639,8.68315531343203,9.88673268190064));
#7228=CARTESIAN_POINT('Ctrl Pts',(7.15119134028659,8.82341656046842,9.82830572643859));
#7229=CARTESIAN_POINT('Ctrl Pts',(6.41157022806713,9.07672862331535,9.69155908354252));
#7230=CARTESIAN_POINT('Ctrl Pts',(6.03624395121828,9.18999945289011,9.61279798983037));
#7231=CARTESIAN_POINT('Ctrl Pts',(5.28680518772518,9.39050807507187,9.44350384379107));
#7232=CARTESIAN_POINT('Ctrl Pts',(4.91193913605487,9.47807443933602,9.35282484136955));
#7233=CARTESIAN_POINT('Ctrl Pts',(3.78601706885828,9.70796487519961,9.06874336660609));
#7234=CARTESIAN_POINT('Ctrl Pts',(3.03362219917569,9.81784991817562,8.86354442007235));
#7235=CARTESIAN_POINT('Ctrl Pts',(1.90012638124304,9.92742805349748,8.54552077981019));
#7236=CARTESIAN_POINT('Ctrl Pts',(1.52148656713009,9.95463063545181,8.4377136379673));
#7237=CARTESIAN_POINT('Ctrl Pts',(0.762253747142684,9.99091801432738,8.22004456397749));
#7238=CARTESIAN_POINT('Ctrl Pts',(0.380054916719888,10.,8.10971233032629));
#7239=CARTESIAN_POINT('Ctrl Pts',(0.,10.,8.));
#7240=CARTESIAN_POINT('Origin',(-4.8710921181488E-16,-8.,8.));
#7241=CARTESIAN_POINT('Origin',(23.0198096393687,-8.,8.));
#7242=CARTESIAN_POINT('Ctrl Pts',(7.46595409979742,6.65278372912403,11.9999659823065));
#7243=CARTESIAN_POINT('Ctrl Pts',(7.46181137603258,6.65743228755678,9.99435834176235));
#7244=CARTESIAN_POINT('Ctrl Pts',(8.95919248103908,7.99171094663393,9.99998316436123));
#7245=CARTESIAN_POINT('Ctrl Pts',(7.2050090532042,6.94561778375818,12.0014006149718));
#7246=CARTESIAN_POINT('Ctrl Pts',(7.29338961739188,6.84609954078222,10.1091476443099));
#7247=CARTESIAN_POINT('Ctrl Pts',(8.64603010975786,8.16742618260248,10.0006968502176));
#7248=CARTESIAN_POINT('Ctrl Pts',(6.93129022829302,7.21830937991486,11.9573878676915));
#7249=CARTESIAN_POINT('Ctrl Pts',(7.08968233035302,7.06312387610362,10.1923050700163));
#7250=CARTESIAN_POINT('Ctrl Pts',(8.31758857577122,8.33102724263676,9.97868692248085));
#7251=CARTESIAN_POINT('Ctrl Pts',(6.36322946527443,7.7234369320712,11.8062939832124));
#7252=CARTESIAN_POINT('Ctrl Pts',(6.62330289734465,7.50555955075384,10.2799383797216));
#7253=CARTESIAN_POINT('Ctrl Pts',(7.63591040831743,8.63410122162527,9.90313394764094));
#7254=CARTESIAN_POINT('Ctrl Pts',(6.0676798404454,7.95720201860455,11.6989395444534));
#7255=CARTESIAN_POINT('Ctrl Pts',(6.36270324053587,7.73143421140555,10.2890080329594));
#7256=CARTESIAN_POINT('Ctrl Pts',(7.28124840537636,8.77435822208396,9.8494541734595));
#7257=CARTESIAN_POINT('Ctrl Pts',(5.47010836911268,8.37924322604346,11.4434059485407));
#7258=CARTESIAN_POINT('Ctrl Pts',(5.80819530329405,8.15710830657298,10.2436830242621));
#7259=CARTESIAN_POINT('Ctrl Pts',(6.56415809876884,9.02757824037212,9.72168360055666));
#7260=CARTESIAN_POINT('Ctrl Pts',(5.16605083626499,8.56956461250842,11.2947420399208));
#7261=CARTESIAN_POINT('Ctrl Pts',(5.51310144140328,8.36060172136931,10.1925886394282));
#7262=CARTESIAN_POINT('Ctrl Pts',(6.19928698920683,9.14176835009192,9.64735037171788));
#7263=CARTESIAN_POINT('Ctrl Pts',(4.54664343995125,8.91367221299836,10.9663084668338));
#7264=CARTESIAN_POINT('Ctrl Pts',(4.89532112501463,8.73555397522188,10.0437605916743));
#7265=CARTESIAN_POINT('Ctrl Pts',(5.45599414260708,9.34822738370456,9.48313222005185));
#7266=CARTESIAN_POINT('Ctrl Pts',(4.23052411852774,9.06774230389022,10.7859725905476));
#7267=CARTESIAN_POINT('Ctrl Pts',(4.5709050130387,8.9097084091423,9.94694323658702));
#7268=CARTESIAN_POINT('Ctrl Pts',(5.07664912268078,9.44066656892447,9.39296418997048));
#7269=CARTESIAN_POINT('Ctrl Pts',(3.26891873105192,9.47624976235846,10.2106353565519));
#7270=CARTESIAN_POINT('Ctrl Pts',(3.58252292320737,9.36878727249013,9.60992785891922));
#7271=CARTESIAN_POINT('Ctrl Pts',(3.92271663488453,9.68576304806697,9.1052966773183));
#7272=CARTESIAN_POINT('Ctrl Pts',(2.62559783884422,9.67195583771219,9.79164439618922));
#7273=CARTESIAN_POINT('Ctrl Pts',(2.88161358543654,9.60711253457495,9.32052272371477));
#7274=CARTESIAN_POINT('Ctrl Pts',(3.1507288339645,9.80318182826186,8.89580416339016));
#7275=CARTESIAN_POINT('Ctrl Pts',(1.32434891203353,9.93411262756739,8.91760334235447));
#7276=CARTESIAN_POINT('Ctrl Pts',(1.46612043782459,9.9184689874319,8.69236195992552));
#7277=CARTESIAN_POINT('Ctrl Pts',(1.58922406203033,9.96046940770512,8.45879148701049));
#7278=CARTESIAN_POINT('Ctrl Pts',(0.664585080193226,10.,8.46043776212904));
#7279=CARTESIAN_POINT('Ctrl Pts',(0.731002622520191,10.,8.34530575506384));
#7280=CARTESIAN_POINT('Ctrl Pts',(0.79752291803651,10.,8.23021899751621));
#7281=CARTESIAN_POINT('Ctrl Pts',(1.07753648825376E-35,10.,8.));
#7282=CARTESIAN_POINT('Ctrl Pts',(1.07753648825376E-35,10.,8.));
#7283=CARTESIAN_POINT('Ctrl Pts',(1.07753648825376E-35,10.,8.));
#7284=CARTESIAN_POINT('Origin',(23.0198096393687,-30.,8.));
#7285=CARTESIAN_POINT('Origin',(1.76944146100923,-24.3059810077445,8.));
#7286=CARTESIAN_POINT('Origin',(7.72740661031253,-2.07055236082019,8.));
#7287=CARTESIAN_POINT('Origin',(-2.62535519378845,-40.7075854123829,8.));
#7288=CARTESIAN_POINT('Ctrl Pts',(-10.038209642496,-6.58550840389661,9.99998316436182));
#7289=CARTESIAN_POINT('Ctrl Pts',(-8.36174489807087,-5.48442051636901,9.99435800706184));
#7290=CARTESIAN_POINT('Ctrl Pts',(-8.35842653183974,-5.48969106142489,12.0000850216378));
#7291=CARTESIAN_POINT('Ctrl Pts',(-10.1268851410615,-6.23753833216136,10.0006968502054));
#7292=CARTESIAN_POINT('Ctrl Pts',(-8.50039843904348,-5.27291666647825,10.1091539159912));
#7293=CARTESIAN_POINT('Ctrl Pts',(-8.57374963798823,-5.1618393734599,12.0015162133387));
#7294=CARTESIAN_POINT('Ctrl Pts',(-10.1999047059325,-5.87794510201831,9.97868692247048));
#7295=CARTESIAN_POINT('Ctrl Pts',(-8.6573118794847,-5.01998806659582,10.1923170765812));
#7296=CARTESIAN_POINT('Ctrl Pts',(-8.76630821829894,-4.82686416035968,11.9574988119276));
#7297=CARTESIAN_POINT('Ctrl Pts',(-10.3162203971305,-5.14105323712323,9.90313394764108));
#7298=CARTESIAN_POINT('Ctrl Pts',(-8.96397867699314,-4.45500100614754,10.2799584618669));
#7299=CARTESIAN_POINT('Ctrl Pts',(-9.1072016651553,-4.14741471865905,11.8063951598433));
#7300=CARTESIAN_POINT('Ctrl Pts',(-10.3599049752557,-4.76217486595153,9.84945417345977));
#7301=CARTESIAN_POINT('Ctrl Pts',(-9.11471603103977,-4.14482487528738,10.2890308821851));
#7302=CARTESIAN_POINT('Ctrl Pts',(-9.25650767056149,-3.80142989829907,11.6990353645558));
#7303=CARTESIAN_POINT('Ctrl Pts',(-10.4189001022453,-4.00398065568352,9.721683600557));
#7304=CARTESIAN_POINT('Ctrl Pts',(-9.3823816234562,-3.49904576722659,10.2437089713902));
#7305=CARTESIAN_POINT('Ctrl Pts',(-9.50950469399203,-3.11498392064292,11.4434912150781));
#7306=CARTESIAN_POINT('Ctrl Pts',(-10.4347636861683,-3.62198765253324,9.64735037171816));
#7307=CARTESIAN_POINT('Ctrl Pts',(-9.50257136926293,-3.16134167300405,10.1926151994274));
#7308=CARTESIAN_POINT('Ctrl Pts',(-9.61464424937305,-2.77202715941802,11.2948219712105));
#7309=CARTESIAN_POINT('Ctrl Pts',(-10.4418094540168,-2.85058636557395,9.48313222005232));
#7310=CARTESIAN_POINT('Ctrl Pts',(-9.70486490881434,-2.46757137018015,10.0437869313745));
#7311=CARTESIAN_POINT('Ctrl Pts',(-9.78671026371757,-2.08466339996095,10.9663778363833));
#7312=CARTESIAN_POINT('Ctrl Pts',(-10.4329171345597,-2.46024219210386,9.39296418997138));
#7313=CARTESIAN_POINT('Ctrl Pts',(-9.78912496618977,-2.10913674788569,9.94696884746788));
#7314=CARTESIAN_POINT('Ctrl Pts',(-9.85371162411618,-1.73943985085122,10.7860367058016));
#7315=CARTESIAN_POINT('Ctrl Pts',(-10.3710024490938,-1.28219336365977,9.10529667731764));
#7316=CARTESIAN_POINT('Ctrl Pts',(-9.97676127425813,-1.03561990945101,9.60995022839333));
#7317=CARTESIAN_POINT('Ctrl Pts',(-9.99941461087311,-0.704872753911718,
10.2106832300891));
#7318=CARTESIAN_POINT('Ctrl Pts',(-10.2846151359094,-0.506120192602798,
8.89580416339026));
#7319=CARTESIAN_POINT('Ctrl Pts',(-10.0255633361174,-0.29691220283424,9.32054117497725));
#7320=CARTESIAN_POINT('Ctrl Pts',(-10.0219463652807,-0.0328249135895384,
9.79168270706518));
#7321=CARTESIAN_POINT('Ctrl Pts',(-10.032396097053,1.04288661560029,8.45879148701088));
#7322=CARTESIAN_POINT('Ctrl Pts',(-9.95996217948876,1.15092964781065,8.69237184195042));
#7323=CARTESIAN_POINT('Ctrl Pts',(-9.93838086697549,1.29192649972561,8.91762214995515));
#7324=CARTESIAN_POINT('Ctrl Pts',(-9.8656723829824,1.81784246744332,8.23021899754132));
#7325=CARTESIAN_POINT('Ctrl Pts',(-9.84845494002237,1.88209883934655,8.34531059201747));
#7326=CARTESIAN_POINT('Ctrl Pts',(-9.83126409379134,1.94625595090589,8.4604474397326));
#7327=CARTESIAN_POINT('Ctrl Pts',(-9.65925826289068,2.58819045102525,8.));
#7328=CARTESIAN_POINT('Ctrl Pts',(-9.65925826289068,2.58819045102525,8.));
#7329=CARTESIAN_POINT('Ctrl Pts',(-9.65925826289068,2.58819045102525,8.));
#7330=CARTESIAN_POINT('Ctrl Pts',(-10.0423545251959,-6.56895087439983,10.));
#7331=CARTESIAN_POINT('Ctrl Pts',(-10.1408406688832,-6.17990680833961,10.));
#7332=CARTESIAN_POINT('Ctrl Pts',(-10.2162788692254,-5.79126062750106,9.97233221567646));
#7333=CARTESIAN_POINT('Ctrl Pts',(-10.3327502239336,-5.01321293394617,9.88673268190063));
#7334=CARTESIAN_POINT('Ctrl Pts',(-10.3736304459015,-4.62385215559531,9.82830572643859));
#7335=CARTESIAN_POINT('Ctrl Pts',(-10.4268830795136,-3.8438710354149,9.69155908354253));
#7336=CARTESIAN_POINT('Ctrl Pts',(-10.4391527105892,-3.45201704337316,9.61279798983037));
#7337=CARTESIAN_POINT('Ctrl Pts',(-10.4388601420181,-2.67621933636512,9.44350384379107));
#7338=CARTESIAN_POINT('Ctrl Pts',(-10.4264202812404,-2.29146269287581,9.35282484136955));
#7339=CARTESIAN_POINT('Ctrl Pts',(-10.3570673161662,-1.14440546669344,9.0687433666061));
#7340=CARTESIAN_POINT('Ctrl Pts',(-10.2684739953883,-0.389207488605518,
8.86354442007235));
#7341=CARTESIAN_POINT('Ctrl Pts',(-10.0809480410673,0.734026304274402,8.54552077981019));
#7342=CARTESIAN_POINT('Ctrl Pts',(-10.0092245223922,1.10680482587314,8.4377136379673));
#7343=CARTESIAN_POINT('Ctrl Pts',(-9.84777152533679,1.8495592796151,8.22004456397749));
#7344=CARTESIAN_POINT('Ctrl Pts',(-9.75762371352207,2.2210855915595,8.10971233033392));
#7345=CARTESIAN_POINT('Ctrl Pts',(-9.65925826289068,2.58819045102525,8.));
#7346=CARTESIAN_POINT('Origin',(-10.352761804101,-38.6370330515627,8.));
#7347=CARTESIAN_POINT('Origin',(-18.0801684144135,-36.5664806907425,8.));
#7348=CARTESIAN_POINT('Origin',(-7.72740661031254,2.0705523608202,8.));
#7349=CARTESIAN_POINT('Origin',(80.,0.,-28.));
#7350=CARTESIAN_POINT('Origin',(80.,-8.,-28.));
#7351=CARTESIAN_POINT('Origin',(80.,8.,-28.));
#7352=CARTESIAN_POINT('Origin',(0.,8.,-28.));
#7353=CARTESIAN_POINT('Origin',(54.,8.,-28.));
#7354=CARTESIAN_POINT('Origin',(23.0198096393687,-8.,-28.));
#7355=CARTESIAN_POINT('Origin',(54.,-8.,-28.));
#7356=CARTESIAN_POINT('Origin',(54.,8.,-23.));
#7357=CARTESIAN_POINT('Origin',(49.,8.,-23.));
#7358=CARTESIAN_POINT('Origin',(54.,-8.,-23.));
#7359=CARTESIAN_POINT('Origin',(49.,-8.,-23.));
#7360=CARTESIAN_POINT('Origin',(49.,8.,-10.));
#7361=CARTESIAN_POINT('Origin',(49.,8.,-12.));
#7362=CARTESIAN_POINT('Origin',(49.,-8.,30.));
#7363=CARTESIAN_POINT('Origin',(49.,-8.,-12.));
#7364=CARTESIAN_POINT('Origin',(45.,10.,-12.));
#7365=CARTESIAN_POINT('Origin',(45.,8.,-12.));
#7366=CARTESIAN_POINT('Origin',(45.,-8.,-12.));
#7367=CARTESIAN_POINT('Origin',(45.,8.,-12.));
#7368=CARTESIAN_POINT('Origin',(45.,8.,-8.));
#7369=CARTESIAN_POINT('Origin',(45.,-8.,-12.));
#7370=CARTESIAN_POINT('Origin',(45.,-8.,-8.));
#7371=CARTESIAN_POINT('Origin',(0.,8.,-8.));
#7372=CARTESIAN_POINT('Ctrl Pts',(0.,10.,-8.));
#7373=CARTESIAN_POINT('Ctrl Pts',(0.21283996478035,10.,-8.06144156707443));
#7374=CARTESIAN_POINT('Ctrl Pts',(0.4262133032106,9.99718006517799,-8.12303992303043));
#7375=CARTESIAN_POINT('Ctrl Pts',(0.63952603930531,9.99149862373395,-8.18448908348713));
#7376=CARTESIAN_POINT('Ctrl Pts',(0.806878166272437,9.98704131224235,-8.23269833667588));
#7377=CARTESIAN_POINT('Ctrl Pts',(0.974192987912469,9.98082375407732,-8.28081555193822));
#7378=CARTESIAN_POINT('Ctrl Pts',(1.14118650650328,9.97284817866079,-8.32869315474917));
#7379=CARTESIAN_POINT('Ctrl Pts',(1.41442329560585,9.95979844693199,-8.40703106015045));
#7380=CARTESIAN_POINT('Ctrl Pts',(1.68739639326401,9.94202171183076,-8.48489994346883));
#7381=CARTESIAN_POINT('Ctrl Pts',(1.96017979151534,9.91942459279275,-8.56202062209405));
#7382=CARTESIAN_POINT('Ctrl Pts',(2.06661525717798,9.91060757935695,-8.59211180577427));
#7383=CARTESIAN_POINT('Ctrl Pts',(2.17302164588681,9.90105623937531,-8.62208885095276));
#7384=CARTESIAN_POINT('Ctrl Pts',(2.2794025303324,9.89076326460884,-8.65193418212132));
#7385=CARTESIAN_POINT('Ctrl Pts',(2.30959079625838,9.887842372749,-8.66040354951436));
#7386=CARTESIAN_POINT('Ctrl Pts',(2.33977974216733,9.88486148480699,-8.66886307566744));
#7387=CARTESIAN_POINT('Ctrl Pts',(2.3699680394493,9.88182053327789,-8.67731195215625));
#7388=CARTESIAN_POINT('Ctrl Pts',(2.60220683799433,9.8584264702423,-8.74230922267101));
#7389=CARTESIAN_POINT('Ctrl Pts',(2.83459916520224,9.83150383039383,-8.80676897495569));
#7390=CARTESIAN_POINT('Ctrl Pts',(3.06684870944628,9.80084819296531,-8.87031999281874));
#7391=CARTESIAN_POINT('Ctrl Pts',(3.29289063466214,9.77101192643735,-8.93217240451646));
#7392=CARTESIAN_POINT('Ctrl Pts',(3.51879773119167,9.73763927964958,-8.99316350389003));
#7393=CARTESIAN_POINT('Ctrl Pts',(3.74430919491659,9.70058815615854,-9.05296006183168));
#7394=CARTESIAN_POINT('Ctrl Pts',(3.96164829554026,9.66487973706699,-9.11058963821226));
#7395=CARTESIAN_POINT('Ctrl Pts',(4.17862027427997,9.6257545265827,-9.16710931434817));
#7396=CARTESIAN_POINT('Ctrl Pts',(4.39499769774148,9.58313143643332,-9.22223551765105));
#7397=CARTESIAN_POINT('Ctrl Pts',(4.44640094103968,9.57300577249843,-9.23533145712178));
#7398=CARTESIAN_POINT('Ctrl Pts',(4.49777064455629,9.56268291649156,-9.24834883534915));
#7399=CARTESIAN_POINT('Ctrl Pts',(4.54910377883995,9.55216219113866,-9.26128401249424));
#7400=CARTESIAN_POINT('Ctrl Pts',(4.59670393277784,9.54240654006993,-9.27327853478306));
#7401=CARTESIAN_POINT('Ctrl Pts',(4.64432976534029,9.53246904754701,-9.28521680416131));
#7402=CARTESIAN_POINT('Ctrl Pts',(4.69198628933828,9.52234638104957,-9.29709733486223));
#7403=CARTESIAN_POINT('Ctrl Pts',(4.88268243400821,9.48184083610209,-9.34463692044747));
#7404=CARTESIAN_POINT('Ctrl Pts',(5.07273585349363,9.43855777060046,-9.39093663099496));
#7405=CARTESIAN_POINT('Ctrl Pts',(5.26204605452408,9.39237389696166,-9.43572635477248));
#7406=CARTESIAN_POINT('Ctrl Pts',(5.45135625555453,9.34619002332286,-9.48051607854999));
#7407=CARTESIAN_POINT('Ctrl Pts',(5.63992377103605,9.29710539175112,-9.52379633480365));
#7408=CARTESIAN_POINT('Ctrl Pts',(5.82761537190849,9.24496973141032,-9.56526367359599));
#7409=CARTESIAN_POINT('Ctrl Pts',(6.0017388658103,9.19660292494044,-9.60373336472639));
#7410=CARTESIAN_POINT('Ctrl Pts',(6.17530928602799,9.14557355400822,-9.64070509993831));
#7411=CARTESIAN_POINT('Ctrl Pts',(6.34849967657397,9.09158877785136,-9.67587155789363));
#7412=CARTESIAN_POINT('Ctrl Pts',(6.49227413063132,9.04677317523686,-9.70506508461134));
#7413=CARTESIAN_POINT('Ctrl Pts',(6.63578649863589,8.99992038455735,-9.7330140518619));
#7414=CARTESIAN_POINT('Ctrl Pts',(6.77913102959258,8.95084501649208,-9.75952238095208));
#7415=CARTESIAN_POINT('Ctrl Pts',(6.82705860123601,8.93443655498206,-9.76838550138743));
#7416=CARTESIAN_POINT('Ctrl Pts',(6.87489556090825,8.91780410736466,-9.77707420344914));
#7417=CARTESIAN_POINT('Ctrl Pts',(6.92267225370638,8.900932814949,-9.78558675592926));
#7418=CARTESIAN_POINT('Ctrl Pts',(7.02826208232899,8.8636460801317,-9.80440009157212));
#7419=CARTESIAN_POINT('Ctrl Pts',(7.13377131742087,8.82508785857041,-9.82237616418793));
#7420=CARTESIAN_POINT('Ctrl Pts',(7.23918103178142,8.78520631381303,-9.83939178290976));
#7421=CARTESIAN_POINT('Ctrl Pts',(7.33826960340199,8.74771636017827,-9.85538701982521));
#7422=CARTESIAN_POINT('Ctrl Pts',(7.43727103940148,8.7090565798954,-9.87053379453038));
#7423=CARTESIAN_POINT('Ctrl Pts',(7.53613923050785,8.66916680576892,-9.88470078228711));
#7424=CARTESIAN_POINT('Ctrl Pts',(7.62793946795173,8.63212869780502,-9.89785499119271));
#7425=CARTESIAN_POINT('Ctrl Pts',(7.71962524418919,8.59402984758295,-9.91016457273228));
#7426=CARTESIAN_POINT('Ctrl Pts',(7.81112455777423,8.55481220143714,-9.92149650701163));
#7427=CARTESIAN_POINT('Ctrl Pts',(7.83242071210478,8.54568442755471,-9.92413397621027));
#7428=CARTESIAN_POINT('Ctrl Pts',(7.85370659135147,8.53649601348149,-9.92671835540356));
#7429=CARTESIAN_POINT('Ctrl Pts',(7.87498095141589,8.52724616974222,-9.92924772122224));
#7430=CARTESIAN_POINT('Ctrl Pts',(7.90803474685888,8.51287476482515,-9.93317757575689));
#7431=CARTESIAN_POINT('Ctrl Pts',(7.94103969858764,8.49836474728666,-9.93697197572982));
#7432=CARTESIAN_POINT('Ctrl Pts',(7.97398093621393,8.48371800839878,-9.94062280955171));
#7433=CARTESIAN_POINT('Ctrl Pts',(8.10713921252213,8.42451153516385,-9.9553805652962));
#7434=CARTESIAN_POINT('Ctrl Pts',(8.23955047791889,8.36300313693741,-9.96789588233122));
#7435=CARTESIAN_POINT('Ctrl Pts',(8.37100368129355,8.29902072598766,-9.97758707535957));
#7436=CARTESIAN_POINT('Ctrl Pts',(8.5025158548848,8.23500961237769,-9.98728261587992));
#7437=CARTESIAN_POINT('Ctrl Pts',(8.63306909525044,8.16852221503888,-9.99415151076986));
#7438=CARTESIAN_POINT('Ctrl Pts',(8.76245266057622,8.09937778327323,-9.99755974503551));
#7439=CARTESIAN_POINT('Ctrl Pts',(8.82332527562265,8.0668465853048,-9.99916325728931));
#7440=CARTESIAN_POINT('Ctrl Pts',(8.88393898903987,8.03372712800054,-10.));
#7441=CARTESIAN_POINT('Ctrl Pts',(8.94427190999916,8.,-10.));
#7442=CARTESIAN_POINT('Origin',(23.0198096393687,-8.,-8.));
#7443=CARTESIAN_POINT('Origin',(23.0198096393687,-8.,-8.));
#7444=CARTESIAN_POINT('Ctrl Pts',(8.94427190999916,8.,-10.));
#7445=CARTESIAN_POINT('Ctrl Pts',(7.4535599249993,6.66666666666667,-10.));
#7446=CARTESIAN_POINT('Ctrl Pts',(7.4535599249993,6.66666666666667,-12.));
#7447=CARTESIAN_POINT('Ctrl Pts',(8.63559126581112,8.17255772523996,-10.));
#7448=CARTESIAN_POINT('Ctrl Pts',(7.28674859645865,6.85316740868464,-10.1119004423149));
#7449=CARTESIAN_POINT('Ctrl Pts',(7.1963453492561,6.95424130474946,-11.9999999936655));
#7450=CARTESIAN_POINT('Ctrl Pts',(8.3121131913303,8.33340210364555,-9.97809158727753));
#7451=CARTESIAN_POINT('Ctrl Pts',(7.0857578605764,7.06684700154838,-10.1930933295107));
#7452=CARTESIAN_POINT('Ctrl Pts',(6.92676099287817,7.22233683920652,-11.9561831730231));
#7453=CARTESIAN_POINT('Ctrl Pts',(7.63587535845283,8.63406215912108,-9.90314699084021));
#7454=CARTESIAN_POINT('Ctrl Pts',(6.62329565969844,7.50556561411578,-10.2799808570395));
#7455=CARTESIAN_POINT('Ctrl Pts',(6.36322946527443,7.7234369320712,-11.8062939832124));
#7456=CARTESIAN_POINT('Ctrl Pts',(7.2812158082226,8.77432121126777,-9.84946977287322));
#7457=CARTESIAN_POINT('Ctrl Pts',(6.36269523253062,7.73144033956278,-10.2890463036146));
#7458=CARTESIAN_POINT('Ctrl Pts',(6.0676798404454,7.95720201860455,-11.6989395444534));
#7459=CARTESIAN_POINT('Ctrl Pts',(6.5641300432471,9.02754593552104,-9.72170297362382));
#7460=CARTESIAN_POINT('Ctrl Pts',(5.80818652806631,8.15711407220398,-10.2437141637145));
#7461=CARTESIAN_POINT('Ctrl Pts',(5.47010836911268,8.37924322604346,-11.4434059485407));
#7462=CARTESIAN_POINT('Ctrl Pts',(6.19926100338533,9.14173876763111,-9.64737102026923));
#7463=CARTESIAN_POINT('Ctrl Pts',(5.51309261372975,8.36060703660556,-10.1926166741021));
#7464=CARTESIAN_POINT('Ctrl Pts',(5.16605083626499,8.56956461250842,-11.2947420399208));
#7465=CARTESIAN_POINT('Ctrl Pts',(5.45597212807415,9.34820332767296,-9.48315423310803));
#7466=CARTESIAN_POINT('Ctrl Pts',(4.89531257093376,8.73555834498249,-10.0437832244647));
#7467=CARTESIAN_POINT('Ctrl Pts',(4.54664343995125,8.91367221299836,-10.9663084668338));
#7468=CARTESIAN_POINT('Ctrl Pts',(5.0766289420487,9.44064538242793,-9.39298629553885));
#7469=CARTESIAN_POINT('Ctrl Pts',(4.57089679609006,8.90971222415245,-9.9469634911357));
#7470=CARTESIAN_POINT('Ctrl Pts',(4.23052411852774,9.06774230389022,-10.7859725905476));
#7471=CARTESIAN_POINT('Ctrl Pts',(3.92270247763147,9.68574985722747,-9.10531767774583));
#7472=CARTESIAN_POINT('Ctrl Pts',(3.58251566415662,9.36878975994216,-9.60994176359841));
#7473=CARTESIAN_POINT('Ctrl Pts',(3.26891873105192,9.47624976235846,-10.2106353565519));
#7474=CARTESIAN_POINT('Ctrl Pts',(3.1507174065752,9.80317350273003,-8.89582219816542));
#7475=CARTESIAN_POINT('Ctrl Pts',(2.88160777767504,9.6071140055565,-9.32053341119141));
#7476=CARTESIAN_POINT('Ctrl Pts',(2.62559783884422,9.67195583771219,-9.79164439618922));
#7477=CARTESIAN_POINT('Ctrl Pts',(1.5892186944781,9.96046757643772,-8.45880167110642));
#7478=CARTESIAN_POINT('Ctrl Pts',(1.46611730572651,9.91846933304019,-8.69236693608767));
#7479=CARTESIAN_POINT('Ctrl Pts',(1.32434891203353,9.93411262756739,-8.91760334235447));
#7480=CARTESIAN_POINT('Ctrl Pts',(0.797519998304341,10.,-8.23022404894487));
#7481=CARTESIAN_POINT('Ctrl Pts',(0.731001164897924,10.,-8.34530828179051));
#7482=CARTESIAN_POINT('Ctrl Pts',(0.664585080192849,10.,-8.46043776212959));
#7483=CARTESIAN_POINT('Ctrl Pts',(1.07753648825376E-35,10.,-8.));
#7484=CARTESIAN_POINT('Ctrl Pts',(1.07753648825376E-35,10.,-8.));
#7485=CARTESIAN_POINT('Ctrl Pts',(1.07753648825376E-35,10.,-8.));
#7486=CARTESIAN_POINT('Origin',(8.94427190999916,8.,-12.));
#7487=CARTESIAN_POINT('Origin',(23.0198096393687,-30.,-8.));
#7488=CARTESIAN_POINT('Origin',(1.76944146100923,-24.3059810077445,-8.));
#7489=CARTESIAN_POINT('Origin',(0.,0.,-12.));
#7490=CARTESIAN_POINT('Origin',(-10.0423545251959,-6.56895087439983,-12.));
#7491=CARTESIAN_POINT('Origin',(-2.62535519378845,-40.7075854123829,-8.));
#7492=CARTESIAN_POINT('Ctrl Pts',(-8.36862877395289,-5.47412573060034,-12.0001188722594));
#7493=CARTESIAN_POINT('Ctrl Pts',(-8.36852928825905,-5.47406065456325,-10.));
#7494=CARTESIAN_POINT('Ctrl Pts',(-10.0423545251959,-6.56895087439983,-10.));
#7495=CARTESIAN_POINT('Ctrl Pts',(-8.57983705192027,-5.1512387964459,-12.0001154444351));
#7496=CARTESIAN_POINT('Ctrl Pts',(-8.50550690521628,-5.2646728693275,-10.1119069073858));
#7497=CARTESIAN_POINT('Ctrl Pts',(-10.1291400589616,-6.22612704243147,-10.));
#7498=CARTESIAN_POINT('Ctrl Pts',(-8.76902620446576,-4.82144682478795,-11.9562940408389));
#7499=CARTESIAN_POINT('Ctrl Pts',(-8.65989255015849,-5.01523379072277,-10.1931054083213));
#7500=CARTESIAN_POINT('Ctrl Pts',(-10.200781511727,-5.87204162762333,-9.97809158727756));
#7501=CARTESIAN_POINT('Ctrl Pts',(-9.10720166492718,-4.14741471914895,-11.8063951574117));
#7502=CARTESIAN_POINT('Ctrl Pts',(-8.96398266446,-4.45499244724459,-10.2800009404067));
#7503=CARTESIAN_POINT('Ctrl Pts',(-10.3161735940769,-5.14102949167403,-9.90314699084018));
#7504=CARTESIAN_POINT('Ctrl Pts',(-9.25650767032995,-3.80142989885983,-11.6990353622533));
#7505=CARTESIAN_POINT('Ctrl Pts',(-9.11471988127295,-4.14481555522226,-10.2890691536593));
#7506=CARTESIAN_POINT('Ctrl Pts',(-10.3598607887893,-4.7621529586233,-9.84946977287314));
#7507=CARTESIAN_POINT('Ctrl Pts',(-9.50950469377493,-3.1149839212988,-11.4434912130292));
#7508=CARTESIAN_POINT('Ctrl Pts',(-9.38238492417113,-3.49903579951157,-10.2437401110933));
#7509=CARTESIAN_POINT('Ctrl Pts',(-10.4188616368525,-4.00396191724158,-9.72170297362389));
#7510=CARTESIAN_POINT('Ctrl Pts',(-9.61464424917777,-2.77202716009635,-11.2948219692898));
#7511=CARTESIAN_POINT('Ctrl Pts',(-9.50257422100183,-3.16133177106954,-10.1926432341521));
#7512=CARTESIAN_POINT('Ctrl Pts',(-10.4347283860805,-3.6219702086617,-9.64737102026915));
#7513=CARTESIAN_POINT('Ctrl Pts',(-9.78671026356967,-2.08466340065288,-10.9663778347164));
#7514=CARTESIAN_POINT('Ctrl Pts',(-9.70486691749541,-2.46756197702794,-10.0438095639491));
#7515=CARTESIAN_POINT('Ctrl Pts',(-10.4417805198947,-2.85057132732743,-9.48315423310812));
#7516=CARTESIAN_POINT('Ctrl Pts',(-9.85371162399755,-1.73943985153029,-10.7860367042605));
#7517=CARTESIAN_POINT('Ctrl Pts',(-9.78912652600938,-2.10912782389522,-9.94698910171766));
#7518=CARTESIAN_POINT('Ctrl Pts',(-10.4328914468443,-2.46022818257953,-9.39298629553918));
#7519=CARTESIAN_POINT('Ctrl Pts',(-9.9994146108298,-0.704872754544601,-10.2106832289395));
#7520=CARTESIAN_POINT('Ctrl Pts',(-9.97676179901941,-1.03561225412241,-9.60996413263565));
#7521=CARTESIAN_POINT('Ctrl Pts',(-10.3709860435543,-1.28218310284341,-9.10531767774516));
#7522=CARTESIAN_POINT('Ctrl Pts',(-10.0219463652877,-0.0328249141047754,
-9.79168270614615));
#7523=CARTESIAN_POINT('Ctrl Pts',(-10.0255632543393,-0.296906212413206,
-9.32055186205687));
#7524=CARTESIAN_POINT('Ctrl Pts',(-10.2846041364368,-0.506111309397711,
-8.89582219816607));
#7525=CARTESIAN_POINT('Ctrl Pts',(-9.93838086701884,1.29192649944193,-8.91762214950163));
#7526=CARTESIAN_POINT('Ctrl Pts',(-9.95996170279527,1.15093276255534,-8.69237681786647));
#7527=CARTESIAN_POINT('Ctrl Pts',(-10.0323929389604,1.04289132628966,-8.45880167110577));
#7528=CARTESIAN_POINT('Ctrl Pts',(-9.83126409382562,1.94625595077792,-8.4604474395028));
#7529=CARTESIAN_POINT('Ctrl Pts',(-9.84845456277914,1.88210024723749,-8.3453131186297));
#7530=CARTESIAN_POINT('Ctrl Pts',(-9.86567162729979,1.81784528768922,-8.23022404897214));
#7531=CARTESIAN_POINT('Ctrl Pts',(-9.65925826289068,2.58819045102525,-8.));
#7532=CARTESIAN_POINT('Ctrl Pts',(-9.65925826289068,2.58819045102525,-8.));
#7533=CARTESIAN_POINT('Ctrl Pts',(-9.65925826289068,2.58819045102525,-8.));
#7534=CARTESIAN_POINT('Ctrl Pts',(-9.65925826289068,2.58819045102525,-8.));
#7535=CARTESIAN_POINT('Ctrl Pts',(-9.71434529937461,2.3826028320288,-8.06144156712679));
#7536=CARTESIAN_POINT('Ctrl Pts',(-9.76684653524052,2.17577016080905,-8.12303992313113));
#7537=CARTESIAN_POINT('Ctrl Pts',(-9.81656808291557,1.96825541453737,-8.18448908363342));
#7538=CARTESIAN_POINT('Ctrl Pts',(-9.85557656828771,1.80545203606357,-8.23269833677755));
#7539=CARTESIAN_POINT('Ctrl Pts',(-9.89287513061151,1.64222910640599,-8.28081555199389));
#7540=CARTESIAN_POINT('Ctrl Pts',(-9.92839241932418,1.47886152331472,-8.32869315475884));
#7541=CARTESIAN_POINT('Ctrl Pts',(-9.9865062312563,1.21155753295729,-8.40703106014776));
#7542=CARTESIAN_POINT('Ctrl Pts',(-10.0399858601837,0.943284810476372,-8.48489994345202));
#7543=CARTESIAN_POINT('Ctrl Pts',(-10.0887602579555,0.673947716385416,-8.56202062206502));
#7544=CARTESIAN_POINT('Ctrl Pts',(-10.107791202562,0.568856940234897,-8.59211180575455));
#7545=CARTESIAN_POINT('Ctrl Pts',(-10.126105316523,0.463604192569669,-8.62208885094254));
#7546=CARTESIAN_POINT('Ctrl Pts',(-10.1436964653019,0.358184130924323,-8.65193418212102));
#7547=CARTESIAN_POINT('Ctrl Pts',(-10.148688398579,0.328268522773503,-8.66040354951402));
#7548=CARTESIAN_POINT('Ctrl Pts',(-10.1536225560833,0.298336729680905,-8.6688630756671));
#7549=CARTESIAN_POINT('Ctrl Pts',(-10.1584985287406,0.26839001751361,-8.67731195215595));
#7550=CARTESIAN_POINT('Ctrl Pts',(-10.1960094231454,0.0380097350912643,
-8.74230922266695));
#7551=CARTESIAN_POINT('Ctrl Pts',(-10.230151710219,-0.193432107512816,-8.80676897494775));
#7552=CARTESIAN_POINT('Ctrl Pts',(-10.2606512435707,-0.425702203233516,
-8.87031999280698));
#7553=CARTESIAN_POINT('Ctrl Pts',(-10.2903355784068,-0.651764130616837,
-8.93217240449971));
#7554=CARTESIAN_POINT('Ctrl Pts',(-10.3165691359871,-0.87861110605177,-8.99316350386837));
#7555=CARTESIAN_POINT('Ctrl Pts',(-10.3391471606142,-1.10602798937071,-9.05296006180536));
#7556=CARTESIAN_POINT('Ctrl Pts',(-10.3609069748836,-1.32520345863631,-9.11058963818087));
#7557=CARTESIAN_POINT('Ctrl Pts',(-10.3792714039689,-1.5449086460783,-9.16710931431195));
#7558=CARTESIAN_POINT('Ctrl Pts',(-10.3941032585197,-1.76494485509671,-9.22223551761038));
#7559=CARTESIAN_POINT('Ctrl Pts',(-10.3976267565664,-1.81721729007841,-9.23533145709489));
#7560=CARTESIAN_POINT('Ctrl Pts',(-10.4009511009633,-1.86950836518269,-9.24834883533589));
#7561=CARTESIAN_POINT('Ctrl Pts',(-10.4040748534343,-1.92181532947563,-9.26128401249444));
#7562=CARTESIAN_POINT('Ctrl Pts',(-10.4069714445036,-1.97031849579353,-9.27327853478326));
#7563=CARTESIAN_POINT('Ctrl Pts',(-10.4096990363332,-2.01889352978961,-9.28521680416154));
#7564=CARTESIAN_POINT('Ctrl Pts',(-10.4122557073664,-2.06754613598716,-9.29709733486248));
#7565=CARTESIAN_POINT('Ctrl Pts',(-10.4224861494618,-2.26222807356218,-9.34463692044782));
#7566=CARTESIAN_POINT('Ctrl Pts',(-10.4298673632025,-2.45700806149994,-9.39093663099528));
#7567=CARTESIAN_POINT('Ctrl Pts',(-10.4342542523557,-2.65182093992959,-9.43572635477272));
#7568=CARTESIAN_POINT('Ctrl Pts',(-10.4386411415088,-2.84663381835925,-9.48051607855016));
#7569=CARTESIAN_POINT('Ctrl Pts',(-10.4400338924942,-3.0414800890347,-9.5237963348037));
#7570=CARTESIAN_POINT('Ctrl Pts',(-10.4382528726121,-3.23626995552021,-9.56526367359598));
#7571=CARTESIAN_POINT('Ctrl Pts',(-10.4366006015294,-3.41697858590976,-9.6037333647265));
#7572=CARTESIAN_POINT('Ctrl Pts',(-10.4322333446654,-3.59784211053558,-9.64070509993859));
#7573=CARTESIAN_POINT('Ctrl Pts',(-10.424913026651,-3.77910346984486,-9.67587155789407));
#7574=CARTESIAN_POINT('Ctrl Pts',(-10.4188360455742,-3.92957805965298,-9.70506508461163));
#7575=CARTESIAN_POINT('Ctrl Pts',(-10.4107234590705,-4.08032675684369,-9.73301405186205));
#7576=CARTESIAN_POINT('Ctrl Pts',(-10.4004205882445,-4.2314885812519,-9.75952238095208));
#7577=CARTESIAN_POINT('Ctrl Pts',(-10.3969757998292,-4.28202988283323,-9.76838550138742));
#7578=CARTESIAN_POINT('Ctrl Pts',(-10.3932912053441,-4.33254163184186,-9.77707420344913));
#7579=CARTESIAN_POINT('Ctrl Pts',(-10.3893603062851,-4.38305698510292,-9.78558675592924));
#7580=CARTESIAN_POINT('Ctrl Pts',(-10.3806727447637,-4.49469944466476,-9.80440009157233));
#7581=CARTESIAN_POINT('Ctrl Pts',(-10.3707361622177,-4.60659314183877,-9.82237616418834));
#7582=CARTESIAN_POINT('Ctrl Pts',(-10.3594955897594,-4.7187332106141,-9.83939178291037));
#7583=CARTESIAN_POINT('Ctrl Pts',(-10.3489290848045,-4.82414853503473,-9.85538701982603));
#7584=CARTESIAN_POINT('Ctrl Pts',(-10.3372100617195,-4.92978246632457,-9.87053379453139));
#7585=CARTESIAN_POINT('Ctrl Pts',(-10.3242684694988,-5.035606038763,-9.88470078228827));
#7586=CARTESIAN_POINT('Ctrl Pts',(-10.3122520542547,-5.13386442670699,-9.89785499119407));
#7587=CARTESIAN_POINT('Ctrl Pts',(-10.2991814159282,-5.23228679391394,-9.91016457273381));
#7588=CARTESIAN_POINT('Ctrl Pts',(-10.2849818436389,-5.33081861772194,-9.92149650701328));
#7589=CARTESIAN_POINT('Ctrl Pts',(-10.2816769414382,-5.35375156490583,-9.92413397621134));
#7590=CARTESIAN_POINT('Ctrl Pts',(-10.2783108059237,-5.3766902819571,-9.92671835540409));
#7591=CARTESIAN_POINT('Ctrl Pts',(-10.2748823525246,-5.39963377150023,-9.92924772122223));
#7592=CARTESIAN_POINT('Ctrl Pts',(-10.2695555931287,-5.43528087947289,-9.93317757575688));
#7593=CARTESIAN_POINT('Ctrl Pts',(-10.2640823025385,-5.47091668362685,-9.93697197572981));
#7594=CARTESIAN_POINT('Ctrl Pts',(-10.2584604588427,-5.50652633077284,-9.9406228095517));
#7595=CARTESIAN_POINT('Ctrl Pts',(-10.2357352951814,-5.65047111172067,-9.95538056529732));
#7596=CARTESIAN_POINT('Ctrl Pts',(-10.2105933020697,-5.79429011756483,-9.96789588233314));
#7597=CARTESIAN_POINT('Ctrl Pts',(-10.1828136314758,-5.93782402816916,-9.9775870753618));
#7598=CARTESIAN_POINT('Ctrl Pts',(-10.1550214988549,-6.08142232843084,-9.98728261588294));
#7599=CARTESIAN_POINT('Ctrl Pts',(-10.1245892696446,-6.22473527971416,-9.9941515107729));
#7600=CARTESIAN_POINT('Ctrl Pts',(-10.0912878080822,-6.367606102781,-9.99755974503757));
#7601=CARTESIAN_POINT('Ctrl Pts',(-10.0756200759097,-6.43482422733345,-9.99916325729003));
#7602=CARTESIAN_POINT('Ctrl Pts',(-10.0593171201802,-6.50194452483541,-10.));
#7603=CARTESIAN_POINT('Ctrl Pts',(-10.0423545251959,-6.56895087439983,-10.));
#7604=CARTESIAN_POINT('Origin',(-7.72740661031254,2.0705523608202,-8.));
#7605=CARTESIAN_POINT('Origin',(0.,0.,-25.));
#7606=CARTESIAN_POINT('Origin',(0.,0.,25.));
#7607=CARTESIAN_POINT('Origin',(-10.352761804101,-38.6370330515627,-13.));
#7608=CARTESIAN_POINT('Origin',(-10.352761804101,-38.6370330515627,13.));
#7609=CARTESIAN_POINT('',(0.,0.,0.));
#7610=CARTESIAN_POINT('Origin',(80.,6.93889390390723E-15,2.));
#7611=CARTESIAN_POINT('',(85.,6.32657050433355E-15,2.));
#7612=CARTESIAN_POINT('Origin',(80.,6.93889390390723E-15,2.));
#7613=CARTESIAN_POINT('',(85.,6.32657050433355E-15,-2.));
#7614=CARTESIAN_POINT('',(85.,6.32657050433355E-15,2.));
#7615=CARTESIAN_POINT('Origin',(80.,6.93889390390723E-15,-2.));
#7616=CARTESIAN_POINT('Origin',(0.,0.,2.));
#7617=CARTESIAN_POINT('',(5.,-6.12323399573677E-16,2.));
#7618=CARTESIAN_POINT('Origin',(0.,0.,2.));
#7619=CARTESIAN_POINT('',(5.,-6.12323399573677E-16,-2.));
#7620=CARTESIAN_POINT('',(5.,-6.12323399573677E-16,2.));
#7621=CARTESIAN_POINT('Origin',(0.,0.,-2.));
#7622=CARTESIAN_POINT('Origin',(0.,0.,2.));
#7623=CARTESIAN_POINT('',(0.,10.,2.));
#7624=CARTESIAN_POINT('',(1.22460635382238E-15,-10.,2.));
#7625=CARTESIAN_POINT('Origin',(0.,0.,2.));
#7626=CARTESIAN_POINT('',(0.,10.,-2.));
#7627=CARTESIAN_POINT('',(0.,10.,2.));
#7628=CARTESIAN_POINT('',(1.22460635382238E-15,-10.,-2.));
#7629=CARTESIAN_POINT('Origin',(0.,0.,-2.));
#7630=CARTESIAN_POINT('',(1.22460635382238E-15,-10.,2.));
#7631=CARTESIAN_POINT('Origin',(0.,0.,2.));
#7632=CARTESIAN_POINT('',(80.,-9.99999999999999,2.));
#7633=CARTESIAN_POINT('',(80.,-9.99999999999999,2.));
#7634=CARTESIAN_POINT('',(80.,10.,2.));
#7635=CARTESIAN_POINT('Origin',(80.,6.93889390390723E-15,2.));
#7636=CARTESIAN_POINT('',(0.,10.,2.));
#7637=CARTESIAN_POINT('Origin',(0.,0.,-2.));
#7638=CARTESIAN_POINT('',(80.,10.,-2.));
#7639=CARTESIAN_POINT('',(0.,10.,-2.));
#7640=CARTESIAN_POINT('',(80.,-9.99999999999999,-2.));
#7641=CARTESIAN_POINT('Origin',(80.,6.93889390390723E-15,-2.));
#7642=CARTESIAN_POINT('',(80.,-9.99999999999999,-2.));
#7643=CARTESIAN_POINT('Origin',(80.,-9.99999999999999,2.));
#7644=CARTESIAN_POINT('',(80.,-9.99999999999999,2.));
#7645=CARTESIAN_POINT('Origin',(80.,6.93889390390723E-15,2.));
#7646=CARTESIAN_POINT('',(80.,10.,2.));
#7647=CARTESIAN_POINT('Origin',(0.,10.,2.));
#7648=CARTESIAN_POINT('',(0.,0.,0.));
#7649=CARTESIAN_POINT('Origin',(20.,-26.,-33.));
#7650=CARTESIAN_POINT('',(25.,-26.,-33.));
#7651=CARTESIAN_POINT('',(15.,-26.,-33.));
#7652=CARTESIAN_POINT('Origin',(20.,-26.,-33.));
#7653=CARTESIAN_POINT('Origin',(20.,-26.,-33.));
#7654=CARTESIAN_POINT('',(16.,-26.,-34.));
#7655=CARTESIAN_POINT('',(15.,-26.,-33.));
#7656=CARTESIAN_POINT('Origin',(20.,-26.,-34.));
#7657=CARTESIAN_POINT('Origin',(0.,0.,-33.));
#7658=CARTESIAN_POINT('',(5.,6.12323399573677E-16,-33.));
#7659=CARTESIAN_POINT('',(-5.,-6.12323399573677E-16,-33.));
#7660=CARTESIAN_POINT('Origin',(0.,0.,-33.));
#7661=CARTESIAN_POINT('Origin',(0.,0.,-33.));
#7662=CARTESIAN_POINT('',(-3.99999999999999,-4.8985871965894E-16,-34.));
#7663=CARTESIAN_POINT('',(-5.,-6.12323399573677E-16,-33.));
#7664=CARTESIAN_POINT('Origin',(0.,0.,-34.));
#7665=CARTESIAN_POINT('Origin',(20.,-26.,34.));
#7666=CARTESIAN_POINT('',(25.,-26.,33.));
#7667=CARTESIAN_POINT('Origin',(20.,-26.,33.));
#7668=CARTESIAN_POINT('',(24.,-26.,34.));
#7669=CARTESIAN_POINT('',(24.,-26.,34.));
#7670=CARTESIAN_POINT('Origin',(20.,-26.,34.));
#7671=CARTESIAN_POINT('Origin',(0.,0.,34.));
#7672=CARTESIAN_POINT('',(5.,-6.12323399573677E-16,33.));
#7673=CARTESIAN_POINT('Origin',(0.,0.,33.));
#7674=CARTESIAN_POINT('',(3.99999999999998,-4.89858719658939E-16,34.));
#7675=CARTESIAN_POINT('',(3.99999999999998,-4.89858719658939E-16,34.));
#7676=CARTESIAN_POINT('Origin',(0.,0.,34.));
#7677=CARTESIAN_POINT('Origin',(0.,0.,34.));
#7678=CARTESIAN_POINT('',(5.,-6.12323399573677E-16,22.));
#7679=CARTESIAN_POINT('Origin',(0.,0.,22.));
#7680=CARTESIAN_POINT('',(5.,-6.12323399573677E-16,34.));
#7681=CARTESIAN_POINT('Origin',(0.,0.,34.));
#7682=CARTESIAN_POINT('',(5.,-6.12323399573677E-16,-22.));
#7683=CARTESIAN_POINT('',(5.,-6.12323399573677E-16,34.));
#7684=CARTESIAN_POINT('Origin',(0.,0.,-22.));
#7685=CARTESIAN_POINT('Origin',(20.,-26.,34.));
#7686=CARTESIAN_POINT('',(25.,-26.,22.));
#7687=CARTESIAN_POINT('Origin',(20.,-26.,22.));
#7688=CARTESIAN_POINT('',(25.,-26.,34.));
#7689=CARTESIAN_POINT('Origin',(20.,-26.,34.));
#7690=CARTESIAN_POINT('',(25.,-26.,-22.));
#7691=CARTESIAN_POINT('',(25.,-26.,34.));
#7692=CARTESIAN_POINT('Origin',(20.,-26.,-22.));
#7693=CARTESIAN_POINT('Origin',(-12.6689495444044,0.,22.));
#7694=CARTESIAN_POINT('',(1.26419667377704E-16,16.2875111776015,22.));
#7695=CARTESIAN_POINT('',(-12.6689495444044,2.44580763519679E-16,22.));
#7696=CARTESIAN_POINT('',(-12.6689495444044,2.44580763519679E-16,22.));
#7697=CARTESIAN_POINT('',(20.,-42.,22.));
#7698=CARTESIAN_POINT('',(20.,-42.,22.));
#7699=CARTESIAN_POINT('',(55.,-42.,22.));
#7700=CARTESIAN_POINT('',(55.,-42.,22.));
#7701=CARTESIAN_POINT('',(90.,-35.8285556752037,22.));
#7702=CARTESIAN_POINT('',(90.,-35.8285556752037,22.));
#7703=CARTESIAN_POINT('',(125.,-42.,22.));
#7704=CARTESIAN_POINT('',(125.,-42.,22.));
#7705=CARTESIAN_POINT('',(160.,-42.,22.));
#7706=CARTESIAN_POINT('',(160.,-42.,22.));
#7707=CARTESIAN_POINT('',(160.,-27.,22.));
#7708=CARTESIAN_POINT('',(160.,-27.,22.));
#7709=CARTESIAN_POINT('',(35.,16.2875111776015,22.));
#7710=CARTESIAN_POINT('',(35.,16.2875111776015,22.));
#7711=CARTESIAN_POINT('',(1.26419667377704E-16,16.2875111776015,22.));
#7712=CARTESIAN_POINT('Origin',(-12.6689495444044,0.,-22.));
#7713=CARTESIAN_POINT('',(1.26419667377704E-16,16.2875111776015,-22.));
#7714=CARTESIAN_POINT('',(-12.6689495444044,2.44580763519679E-16,-22.));
#7715=CARTESIAN_POINT('',(-12.6689495444044,2.44580763519679E-16,-22.));
#7716=CARTESIAN_POINT('',(35.,16.2875111776015,-22.));
#7717=CARTESIAN_POINT('',(1.26419667377704E-16,16.2875111776015,-22.));
#7718=CARTESIAN_POINT('',(160.,-27.,-22.));
#7719=CARTESIAN_POINT('',(35.,16.2875111776015,-22.));
#7720=CARTESIAN_POINT('',(160.,-42.,-22.));
#7721=CARTESIAN_POINT('',(160.,-27.,-22.));
#7722=CARTESIAN_POINT('',(125.,-42.,-22.));
#7723=CARTESIAN_POINT('',(160.,-42.,-22.));
#7724=CARTESIAN_POINT('',(90.,-35.8285556752037,-22.));
#7725=CARTESIAN_POINT('',(125.,-42.,-22.));
#7726=CARTESIAN_POINT('',(55.,-42.,-22.));
#7727=CARTESIAN_POINT('',(90.,-35.8285556752037,-22.));
#7728=CARTESIAN_POINT('',(20.,-42.,-22.));
#7729=CARTESIAN_POINT('',(55.,-42.,-22.));
#7730=CARTESIAN_POINT('',(20.,-42.,-22.));
#7731=CARTESIAN_POINT('Origin',(-12.6689495444044,2.44580763519679E-16,
22.));
#7732=CARTESIAN_POINT('',(-12.6689495444044,2.44580763519679E-16,22.));
#7733=CARTESIAN_POINT('',(1.26419667377704E-16,16.2875111776015,22.));
#7734=CARTESIAN_POINT('Origin',(20.,-42.,22.));
#7735=CARTESIAN_POINT('',(20.,-42.,22.));
#7736=CARTESIAN_POINT('Origin',(55.,-42.,22.));
#7737=CARTESIAN_POINT('',(55.,-42.,22.));
#7738=CARTESIAN_POINT('Origin',(90.,-35.8285556752037,22.));
#7739=CARTESIAN_POINT('',(90.,-35.8285556752037,22.));
#7740=CARTESIAN_POINT('Origin',(125.,-42.,22.));
#7741=CARTESIAN_POINT('',(125.,-42.,22.));
#7742=CARTESIAN_POINT('Origin',(160.,-42.,22.));
#7743=CARTESIAN_POINT('',(160.,-42.,22.));
#7744=CARTESIAN_POINT('Origin',(160.,-27.,22.));
#7745=CARTESIAN_POINT('',(160.,-27.,22.));
#7746=CARTESIAN_POINT('Origin',(35.,16.2875111776015,22.));
#7747=CARTESIAN_POINT('',(35.,16.2875111776015,22.));
#7748=CARTESIAN_POINT('Origin',(1.26419667377704E-16,16.2875111776015,22.));
#7749=CARTESIAN_POINT('Origin',(20.,-26.,-34.));
#7750=CARTESIAN_POINT('Origin',(20.,-26.,34.));
#7751=CARTESIAN_POINT('Origin',(0.,0.,-34.));
#7752=CARTESIAN_POINT('Origin',(0.,0.,34.));
#7753=CARTESIAN_POINT('',(0.11182643506261,-5.76334167982517,-30.3315151060526));
#7754=CARTESIAN_POINT('',(0.111826435062603,-5.76334167982517,-35.3315151060526));
#7755=CARTESIAN_POINT('',(0.11182643506261,-5.76334167982518,-124.117480979225));
#7756=CARTESIAN_POINT('',(1.11182643506261,-72.7633416798245,-157.331515106053));
#7757=CARTESIAN_POINT('',(1.11182643506261,-33.8390642460722,-148.117361522534));
#7758=CARTESIAN_POINT('',(1.11182643506261,-75.1116524858088,-237.297041655676));
#7759=CARTESIAN_POINT('',(27.1118264350626,-46.7633416798252,-177.331515106053));
#7760=CARTESIAN_POINT('',(1.11182643506261,22.3123808864206,-148.117361522533));
#7761=CARTESIAN_POINT('',(1.11182643506261,61.236658320175,-157.331515106052));
#7762=CARTESIAN_POINT('',(29.1118264350626,35.2366583201748,-177.331515106053));
#7763=CARTESIAN_POINT('',(1.11182643506261,63.5849691261539,-237.297041655677));
#7764=UNCERTAINTY_MEASURE_WITH_UNIT(LENGTH_MEASURE(0.01),#7784,
'DISTANCE_ACCURACY_VALUE',
'Maximum model space distance between geometric entities at asserted c
onnectivities');
#7765=UNCERTAINTY_MEASURE_WITH_UNIT(LENGTH_MEASURE(0.01),#7784,
'DISTANCE_ACCURACY_VALUE',
'Maximum model space distance between geometric entities at asserted c
onnectivities');
#7766=UNCERTAINTY_MEASURE_WITH_UNIT(LENGTH_MEASURE(0.01),#7784,
'DISTANCE_ACCURACY_VALUE',
'Maximum model space distance between geometric entities at asserted c
onnectivities');
#7767=UNCERTAINTY_MEASURE_WITH_UNIT(LENGTH_MEASURE(0.01),#7784,
'DISTANCE_ACCURACY_VALUE',
'Maximum model space distance between geometric entities at asserted c
onnectivities');
#7768=UNCERTAINTY_MEASURE_WITH_UNIT(LENGTH_MEASURE(0.01),#7784,
'DISTANCE_ACCURACY_VALUE',
'Maximum model space distance between geometric entities at asserted c
onnectivities');
#7769=UNCERTAINTY_MEASURE_WITH_UNIT(LENGTH_MEASURE(0.01),#7784,
'DISTANCE_ACCURACY_VALUE',
'Maximum model space distance between geometric entities at asserted c
onnectivities');
#7770=UNCERTAINTY_MEASURE_WITH_UNIT(LENGTH_MEASURE(0.01),#7784,
'DISTANCE_ACCURACY_VALUE',
'Maximum model space distance between geometric entities at asserted c
onnectivities');
#7771=UNCERTAINTY_MEASURE_WITH_UNIT(LENGTH_MEASURE(0.01),#7784,
'DISTANCE_ACCURACY_VALUE',
'Maximum model space distance between geometric entities at asserted c
onnectivities');
#7772=UNCERTAINTY_MEASURE_WITH_UNIT(LENGTH_MEASURE(0.01),#7784,
'DISTANCE_ACCURACY_VALUE',
'Maximum model space distance between geometric entities at asserted c
onnectivities');
#7773=UNCERTAINTY_MEASURE_WITH_UNIT(LENGTH_MEASURE(0.01),#7784,
'DISTANCE_ACCURACY_VALUE',
'Maximum model space distance between geometric entities at asserted c
onnectivities');
#7774=(
GEOMETRIC_REPRESENTATION_CONTEXT(3)
GLOBAL_UNCERTAINTY_ASSIGNED_CONTEXT((#7764))
GLOBAL_UNIT_ASSIGNED_CONTEXT((#7784,#7786,#7787))
REPRESENTATION_CONTEXT('','3D')
);
#7775=(
GEOMETRIC_REPRESENTATION_CONTEXT(3)
GLOBAL_UNCERTAINTY_ASSIGNED_CONTEXT((#7765))
GLOBAL_UNIT_ASSIGNED_CONTEXT((#7784,#7786,#7787))
REPRESENTATION_CONTEXT('','3D')
);
#7776=(
GEOMETRIC_REPRESENTATION_CONTEXT(3)
GLOBAL_UNCERTAINTY_ASSIGNED_CONTEXT((#7766))
GLOBAL_UNIT_ASSIGNED_CONTEXT((#7784,#7786,#7787))
REPRESENTATION_CONTEXT('','3D')
);
#7777=(
GEOMETRIC_REPRESENTATION_CONTEXT(3)
GLOBAL_UNCERTAINTY_ASSIGNED_CONTEXT((#7767))
GLOBAL_UNIT_ASSIGNED_CONTEXT((#7784,#7786,#7787))
REPRESENTATION_CONTEXT('','3D')
);
#7778=(
GEOMETRIC_REPRESENTATION_CONTEXT(3)
GLOBAL_UNCERTAINTY_ASSIGNED_CONTEXT((#7768))
GLOBAL_UNIT_ASSIGNED_CONTEXT((#7784,#7786,#7787))
REPRESENTATION_CONTEXT('','3D')
);
#7779=(
GEOMETRIC_REPRESENTATION_CONTEXT(3)
GLOBAL_UNCERTAINTY_ASSIGNED_CONTEXT((#7769))
GLOBAL_UNIT_ASSIGNED_CONTEXT((#7784,#7786,#7787))
REPRESENTATION_CONTEXT('','3D')
);
#7780=(
GEOMETRIC_REPRESENTATION_CONTEXT(3)
GLOBAL_UNCERTAINTY_ASSIGNED_CONTEXT((#7770))
GLOBAL_UNIT_ASSIGNED_CONTEXT((#7784,#7786,#7787))
REPRESENTATION_CONTEXT('','3D')
);
#7781=(
GEOMETRIC_REPRESENTATION_CONTEXT(3)
GLOBAL_UNCERTAINTY_ASSIGNED_CONTEXT((#7771))
GLOBAL_UNIT_ASSIGNED_CONTEXT((#7784,#7786,#7787))
REPRESENTATION_CONTEXT('','3D')
);
#7782=(
GEOMETRIC_REPRESENTATION_CONTEXT(3)
GLOBAL_UNCERTAINTY_ASSIGNED_CONTEXT((#7772))
GLOBAL_UNIT_ASSIGNED_CONTEXT((#7784,#7786,#7787))
REPRESENTATION_CONTEXT('','3D')
);
#7783=(
GEOMETRIC_REPRESENTATION_CONTEXT(3)
GLOBAL_UNCERTAINTY_ASSIGNED_CONTEXT((#7773))
GLOBAL_UNIT_ASSIGNED_CONTEXT((#7784,#7786,#7787))
REPRESENTATION_CONTEXT('','3D')
);
#7784=(
LENGTH_UNIT()
NAMED_UNIT(*)
SI_UNIT(.MILLI.,.METRE.)
);
#7785=(
LENGTH_UNIT()
NAMED_UNIT(*)
SI_UNIT($,.METRE.)
);
#7786=(
NAMED_UNIT(*)
PLANE_ANGLE_UNIT()
SI_UNIT($,.RADIAN.)
);
#7787=(
NAMED_UNIT(*)
SI_UNIT($,.STERADIAN.)
SOLID_ANGLE_UNIT()
);
#7788=SHAPE_DEFINITION_REPRESENTATION(#7797,#7818);
#7789=SHAPE_DEFINITION_REPRESENTATION(#7798,#7819);
#7790=SHAPE_DEFINITION_REPRESENTATION(#7799,#7820);
#7791=SHAPE_DEFINITION_REPRESENTATION(#7801,#7821);
#7792=SHAPE_DEFINITION_REPRESENTATION(#7802,#7822);
#7793=SHAPE_DEFINITION_REPRESENTATION(#7803,#7823);
#7794=SHAPE_DEFINITION_REPRESENTATION(#7804,#7824);
#7795=SHAPE_DEFINITION_REPRESENTATION(#7805,#7825);
#7796=SHAPE_DEFINITION_REPRESENTATION(#7806,#7826);
#7797=PRODUCT_DEFINITION_SHAPE('',$,#7828);
#7798=PRODUCT_DEFINITION_SHAPE('',$,#7829);
#7799=PRODUCT_DEFINITION_SHAPE('',$,#7830);
#7800=PRODUCT_DEFINITION_SHAPE($,$,#63);
#7801=PRODUCT_DEFINITION_SHAPE('',$,#7831);
#7802=PRODUCT_DEFINITION_SHAPE('',$,#7832);
#7803=PRODUCT_DEFINITION_SHAPE('',$,#7833);
#7804=PRODUCT_DEFINITION_SHAPE('',$,#7834);
#7805=PRODUCT_DEFINITION_SHAPE('',$,#7835);
#7806=PRODUCT_DEFINITION_SHAPE('',$,#7836);
#7807=PRODUCT_DEFINITION_SHAPE($,$,#64);
#7808=PRODUCT_DEFINITION_SHAPE($,$,#65);
#7809=PRODUCT_DEFINITION_SHAPE($,$,#66);
#7810=PRODUCT_DEFINITION_SHAPE($,$,#67);
#7811=PRODUCT_DEFINITION_SHAPE($,$,#68);
#7812=PRODUCT_DEFINITION_SHAPE($,$,#69);
#7813=PRODUCT_DEFINITION_SHAPE($,$,#70);
#7814=PRODUCT_DEFINITION_SHAPE($,$,#71);
#7815=PRODUCT_DEFINITION_SHAPE($,$,#72);
#7816=PRODUCT_DEFINITION_SHAPE($,$,#73);
#7817=PRODUCT_DEFINITION_SHAPE($,$,#74);
#7818=SHAPE_REPRESENTATION('',(#4249,#4701,#4702,#4703,#4704,#4705,#4706,
#4707,#4708,#4709,#4710,#4711),#7774);
#7819=SHAPE_REPRESENTATION('',(#4250,#4337),#7775);
#7820=SHAPE_REPRESENTATION('',(#4251),#7776);
#7821=SHAPE_REPRESENTATION('',(#4338),#7777);
#7822=SHAPE_REPRESENTATION('',(#4381),#7778);
#7823=SHAPE_REPRESENTATION('',(#4461),#7779);
#7824=SHAPE_REPRESENTATION('',(#4478),#7780);
#7825=SHAPE_REPRESENTATION('',(#4646),#7781);
#7826=SHAPE_REPRESENTATION('',(#4663),#7782);
#7827=PRODUCT_DEFINITION_CONTEXT('part definition',#7856,'design');
#7828=PRODUCT_DEFINITION('MAT-039','MAT-039',#7837,#7827);
#7829=PRODUCT_DEFINITION('Base Frame','Base Frame',#7838,#7827);
#7830=PRODUCT_DEFINITION('Body 1','Body 1',#7839,#7827);
#7831=PRODUCT_DEFINITION('Screw','Screw',#7840,#7827);
#7832=PRODUCT_DEFINITION('Nut','Nut',#7841,#7827);
#7833=PRODUCT_DEFINITION('Link Type 1','Link Type 1',#7842,#7827);
#7834=PRODUCT_DEFINITION('Lever','Lever',#7843,#7827);
#7835=PRODUCT_DEFINITION('Link Type 2','Link Type 2',#7844,#7827);
#7836=PRODUCT_DEFINITION('Cam','Cam',#7845,#7827);
#7837=PRODUCT_DEFINITION_FORMATION('',$,#7858);
#7838=PRODUCT_DEFINITION_FORMATION('',$,#7859);
#7839=PRODUCT_DEFINITION_FORMATION('',$,#7860);
#7840=PRODUCT_DEFINITION_FORMATION('',$,#7861);
#7841=PRODUCT_DEFINITION_FORMATION('',$,#7862);
#7842=PRODUCT_DEFINITION_FORMATION('',$,#7863);
#7843=PRODUCT_DEFINITION_FORMATION('',$,#7864);
#7844=PRODUCT_DEFINITION_FORMATION('',$,#7865);
#7845=PRODUCT_DEFINITION_FORMATION('',$,#7866);
#7846=PRODUCT_RELATED_PRODUCT_CATEGORY('MAT-039','MAT-039',(#7858));
#7847=PRODUCT_RELATED_PRODUCT_CATEGORY('Base Frame','Base Frame',(#7859));
#7848=PRODUCT_RELATED_PRODUCT_CATEGORY('Body 1','Body 1',(#7860));
#7849=PRODUCT_RELATED_PRODUCT_CATEGORY('Screw','Screw',(#7861));
#7850=PRODUCT_RELATED_PRODUCT_CATEGORY('Nut','Nut',(#7862));
#7851=PRODUCT_RELATED_PRODUCT_CATEGORY('Link Type 1','Link Type 1',(#7863));
#7852=PRODUCT_RELATED_PRODUCT_CATEGORY('Lever','Lever',(#7864));
#7853=PRODUCT_RELATED_PRODUCT_CATEGORY('Link Type 2','Link Type 2',(#7865));
#7854=PRODUCT_RELATED_PRODUCT_CATEGORY('Cam','Cam',(#7866));
#7855=APPLICATION_PROTOCOL_DEFINITION('international standard',
'automotive_design',2009,#7856);
#7856=APPLICATION_CONTEXT(
'Core Data for Automotive Mechanical Design Process');
#7857=PRODUCT_CONTEXT('part definition',#7856,'mechanical');
#7858=PRODUCT('MAT-039','MAT-039','STEP AP214',(#7857));
#7859=PRODUCT('Base Frame','Base Frame',$,(#7857));
#7860=PRODUCT('Body 1','Body 1',$,(#7857));
#7861=PRODUCT('Screw','Screw',$,(#7857));
#7862=PRODUCT('Nut','Nut',$,(#7857));
#7863=PRODUCT('Link Type 1','Link Type 1',$,(#7857));
#7864=PRODUCT('Lever','Lever','Lever',(#7857));
#7865=PRODUCT('Link Type 2','Link Type 2',$,(#7857));
#7866=PRODUCT('Cam','Cam',$,(#7857));
#7867=PRESENTATION_STYLE_ASSIGNMENT((#7872));
#7868=PRESENTATION_STYLE_ASSIGNMENT((#7873));
#7869=PRESENTATION_STYLE_ASSIGNMENT((#7874));
#7870=PRESENTATION_STYLE_ASSIGNMENT((#7875));
#7871=PRESENTATION_STYLE_ASSIGNMENT((#7876));
#7872=SURFACE_STYLE_USAGE(.BOTH.,#7877);
#7873=SURFACE_STYLE_USAGE(.BOTH.,#7878);
#7874=SURFACE_STYLE_USAGE(.BOTH.,#7879);
#7875=SURFACE_STYLE_USAGE(.BOTH.,#7880);
#7876=SURFACE_STYLE_USAGE(.BOTH.,#7881);
#7877=SURFACE_SIDE_STYLE('',(#7882));
#7878=SURFACE_SIDE_STYLE('',(#7883));
#7879=SURFACE_SIDE_STYLE('',(#7884));
#7880=SURFACE_SIDE_STYLE('',(#7885));
#7881=SURFACE_SIDE_STYLE('',(#7886));
#7882=SURFACE_STYLE_FILL_AREA(#7887);
#7883=SURFACE_STYLE_FILL_AREA(#7888);
#7884=SURFACE_STYLE_FILL_AREA(#7889);
#7885=SURFACE_STYLE_FILL_AREA(#7890);
#7886=SURFACE_STYLE_FILL_AREA(#7891);
#7887=FILL_AREA_STYLE('Steel - Satin',(#7892));
#7888=FILL_AREA_STYLE('Opaque(61,176,222)',(#7893));
#7889=FILL_AREA_STYLE('Opaque(31,36,43)',(#7894));
#7890=FILL_AREA_STYLE('Opaque(97,158,199)',(#7895));
#7891=FILL_AREA_STYLE('Opaque(227,224,212)',(#7896));
#7892=FILL_AREA_STYLE_COLOUR('Steel - Satin',#7897);
#7893=FILL_AREA_STYLE_COLOUR('Opaque(61,176,222)',#7898);
#7894=FILL_AREA_STYLE_COLOUR('Opaque(31,36,43)',#7899);
#7895=FILL_AREA_STYLE_COLOUR('Opaque(97,158,199)',#7900);
#7896=FILL_AREA_STYLE_COLOUR('Opaque(227,224,212)',#7901);
#7897=COLOUR_RGB('Steel - Satin',0.627450980392157,0.627450980392157,0.627450980392157);
#7898=COLOUR_RGB('Opaque(61,176,222)',0.23921568627451,0.690196078431373,
0.870588235294118);
#7899=COLOUR_RGB('Opaque(31,36,43)',0.12156862745098,0.141176470588235,
0.168627450980392);
#7900=COLOUR_RGB('Opaque(97,158,199)',0.380392156862745,0.619607843137255,
0.780392156862745);
#7901=COLOUR_RGB('Opaque(227,224,212)',0.890196078431372,0.87843137254902,
0.831372549019608);
ENDSEC;
END-ISO-10303-21;
